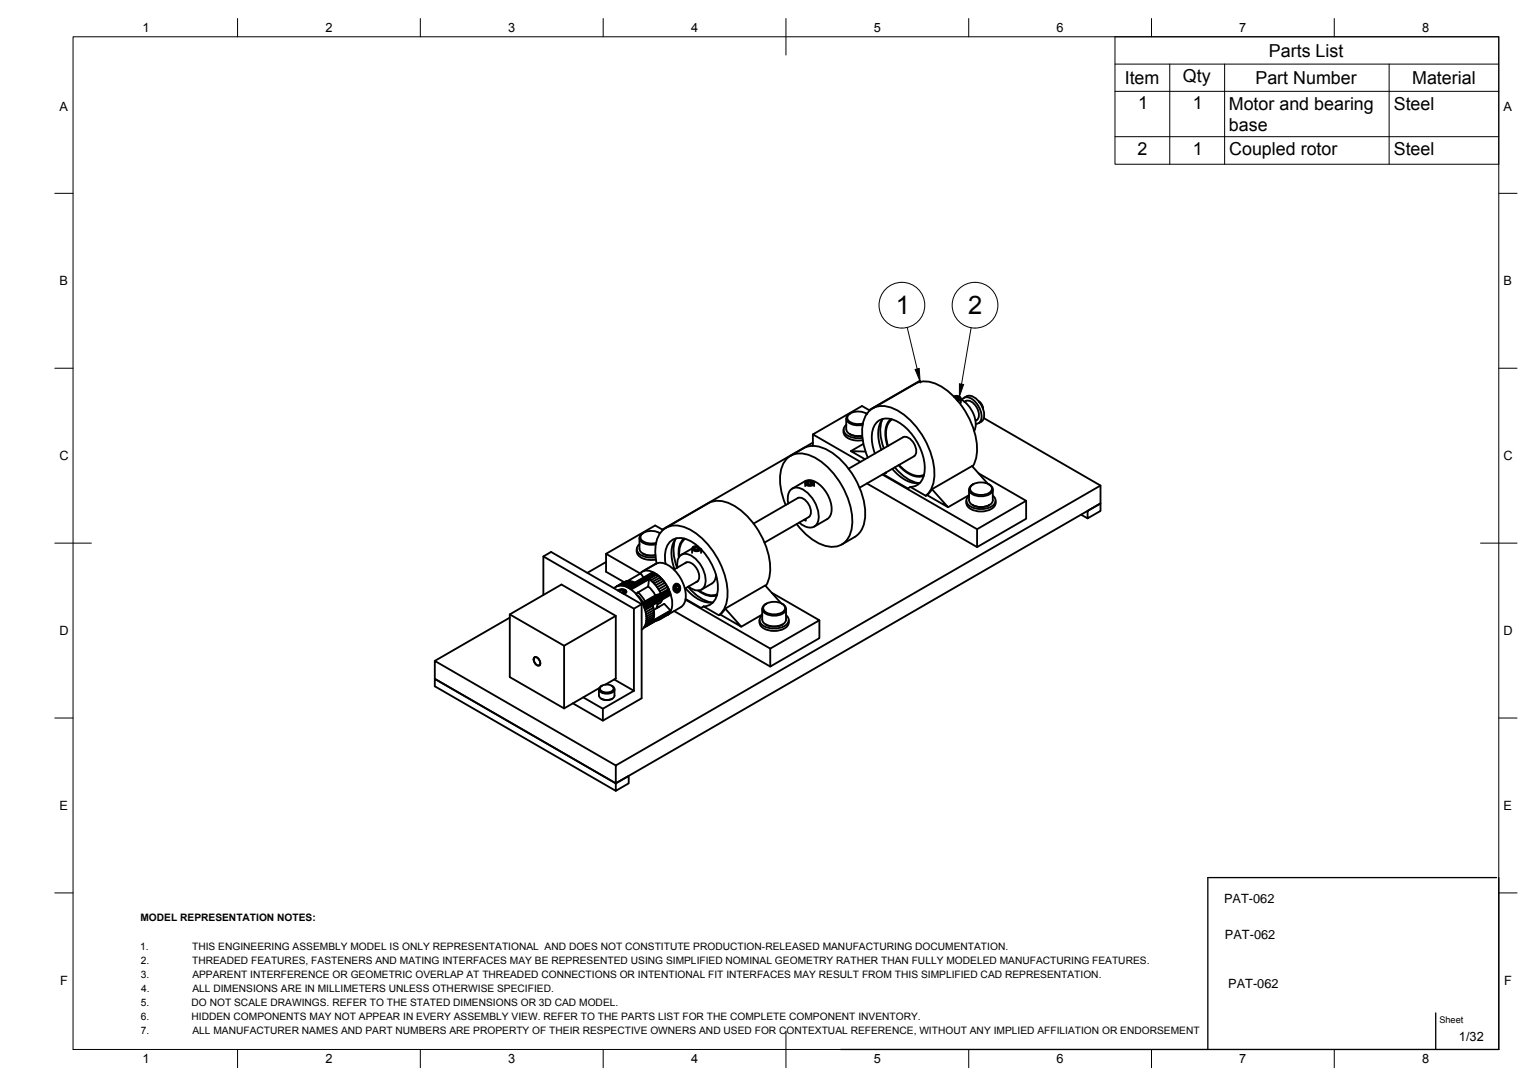
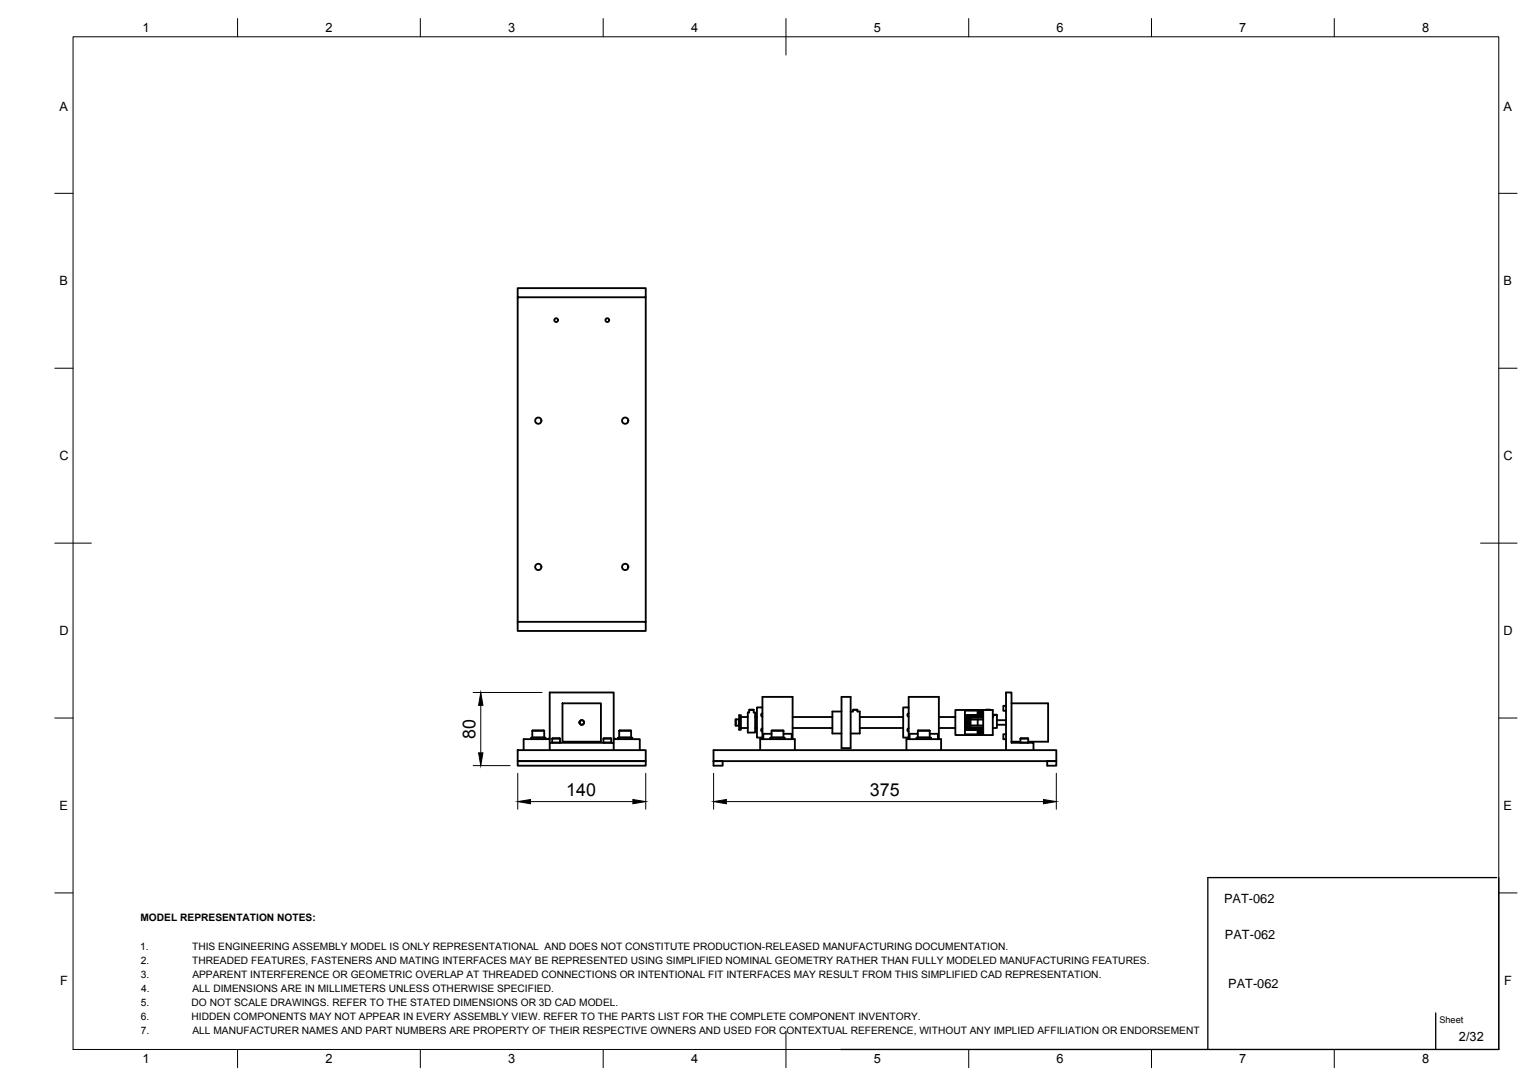
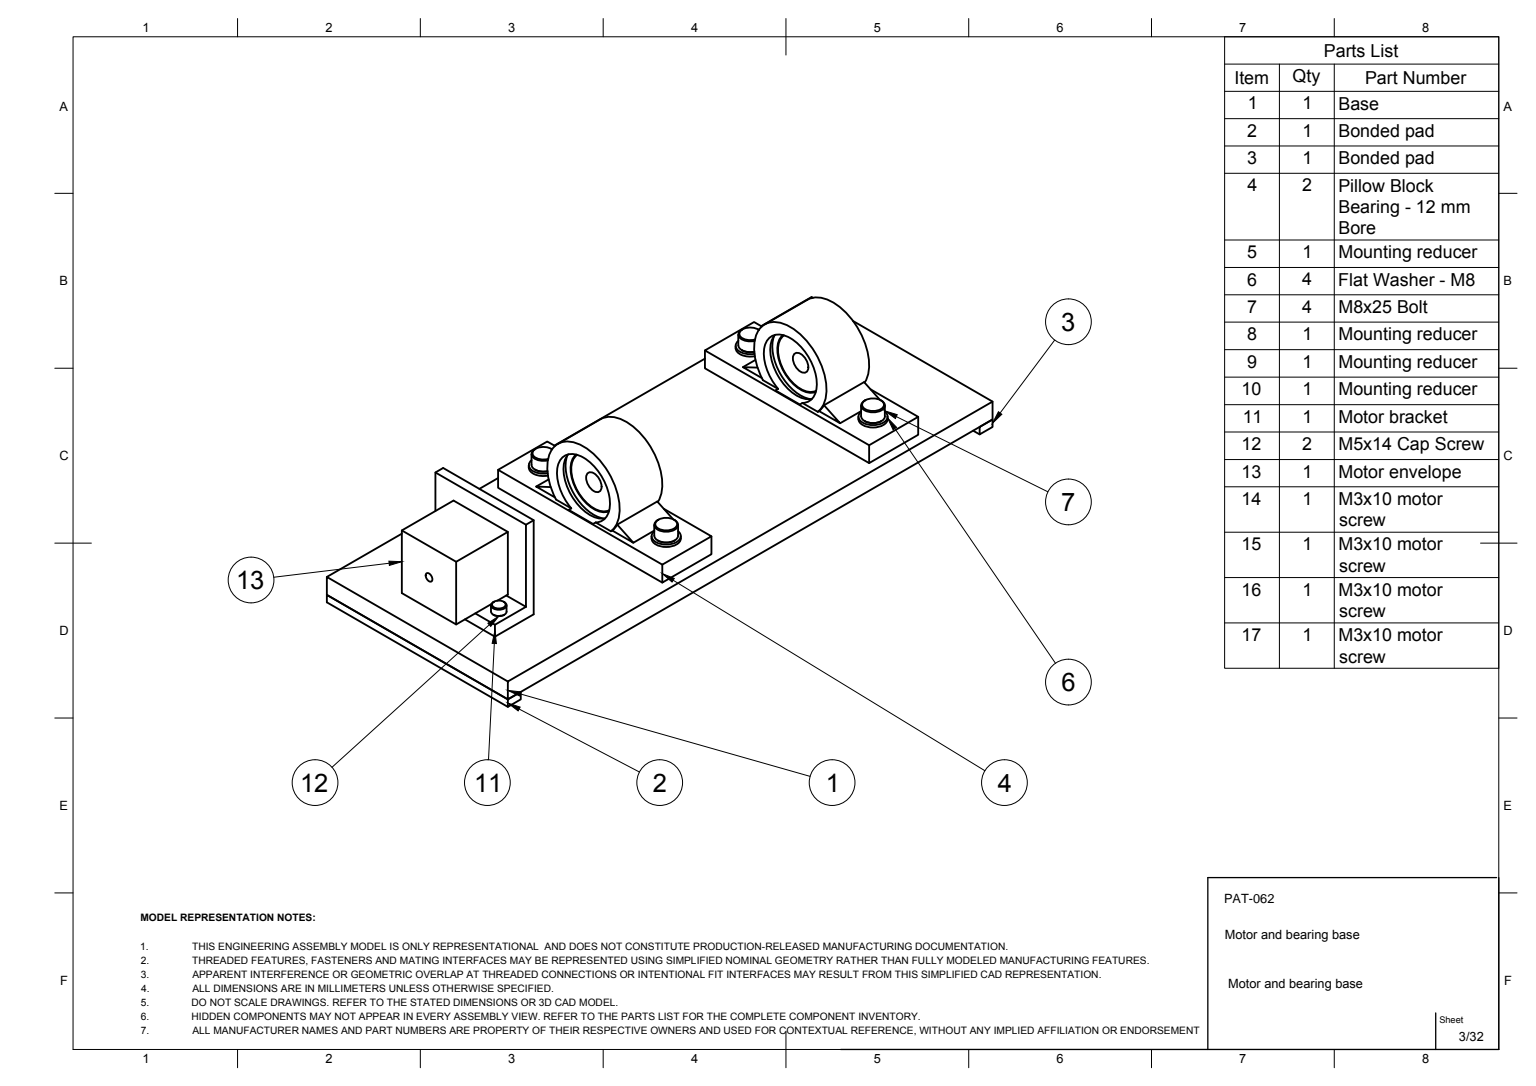
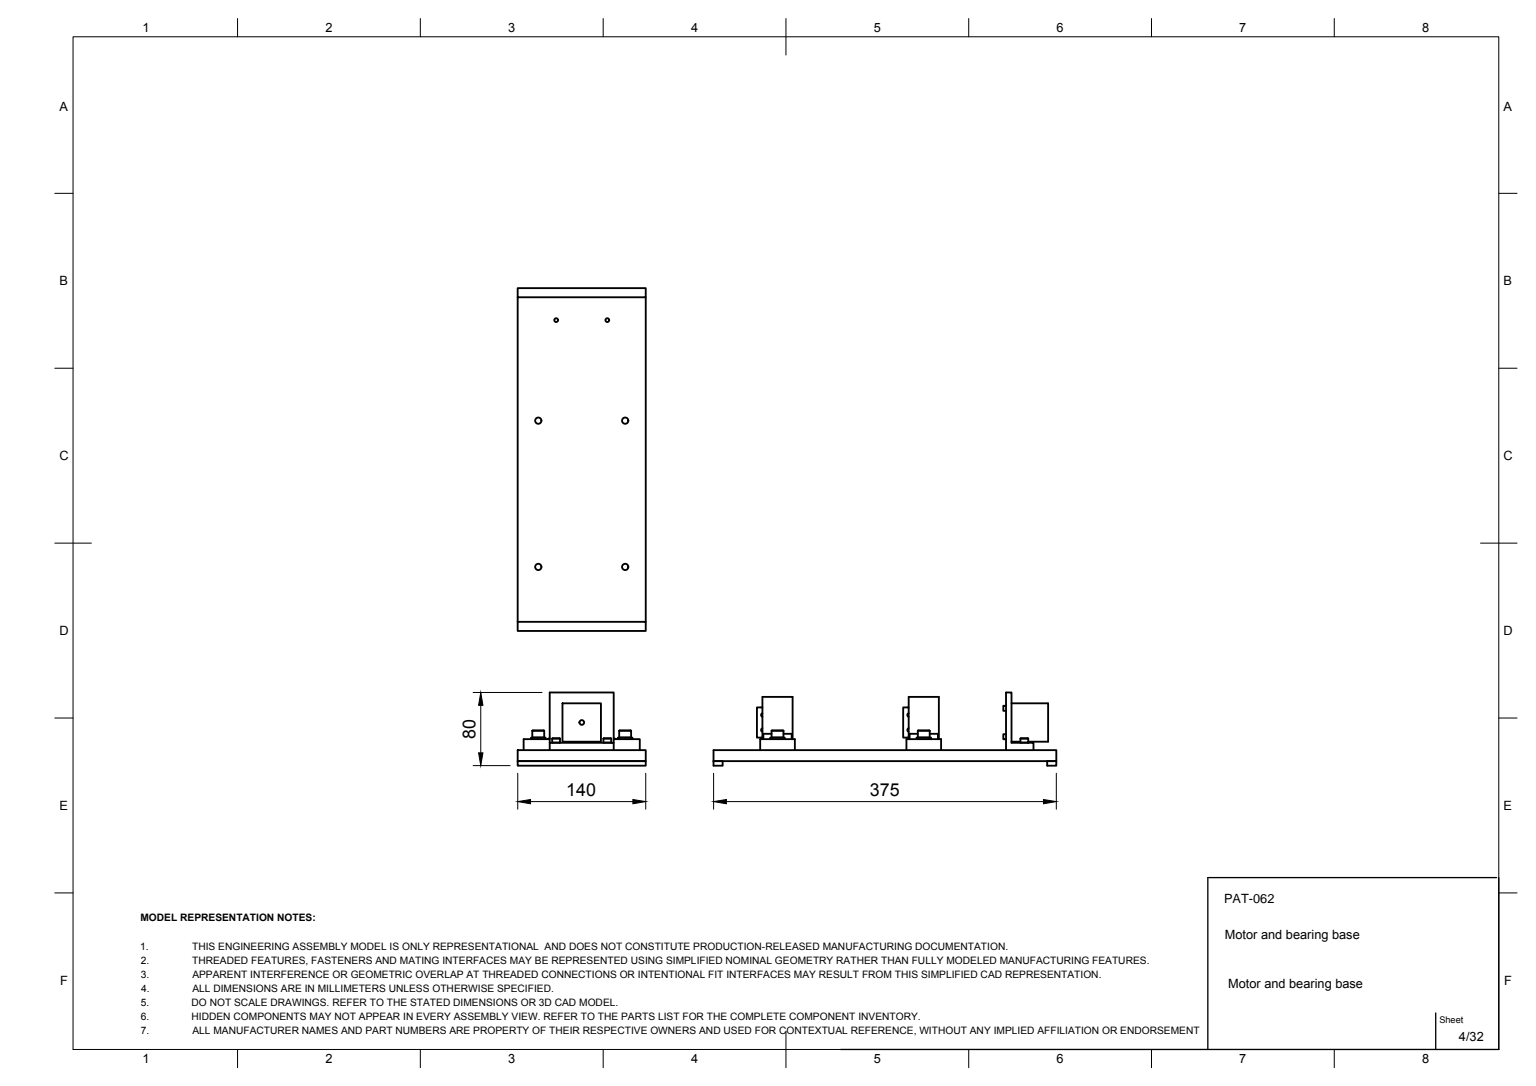
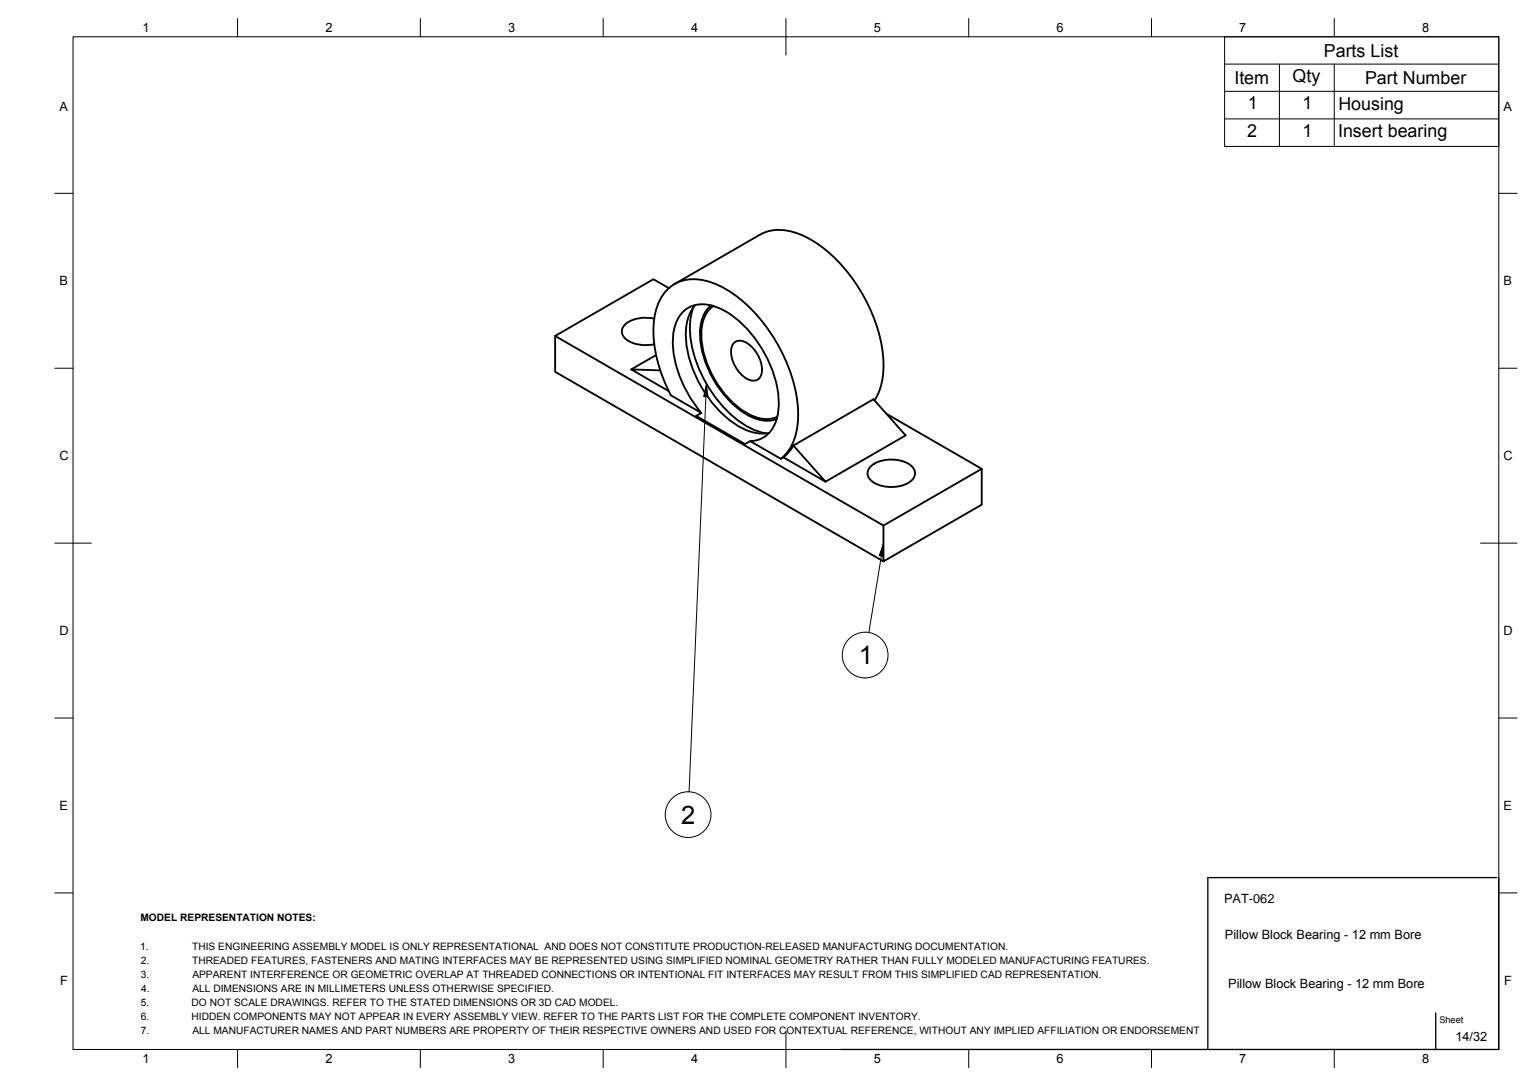
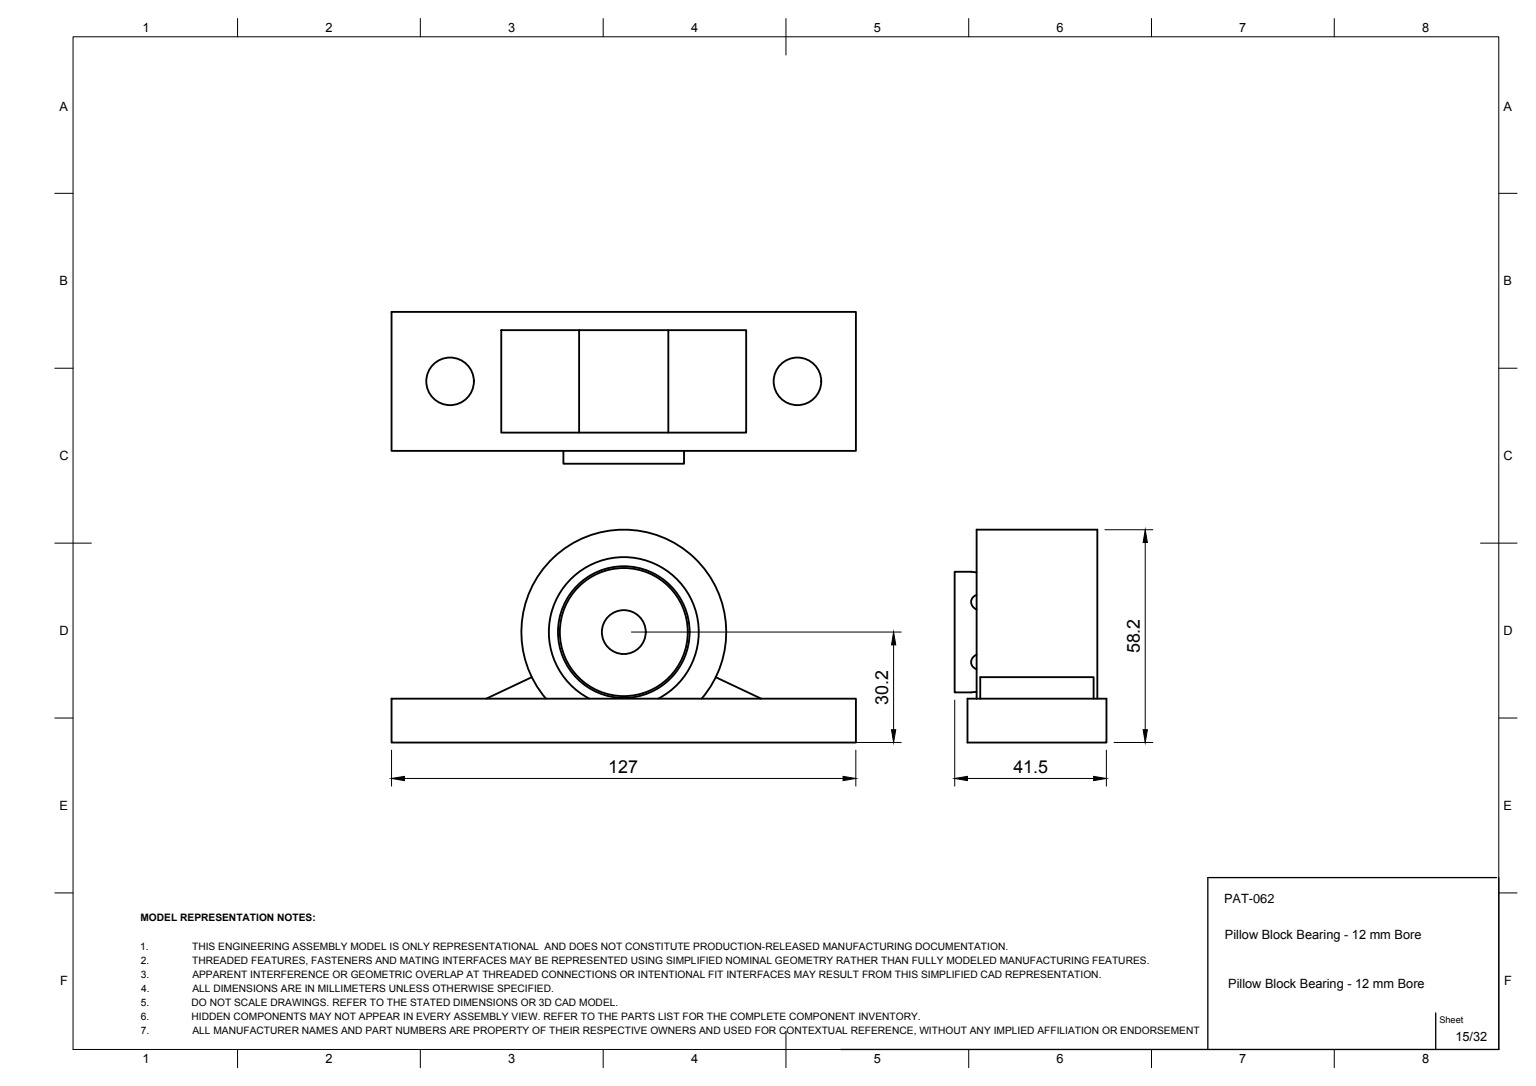
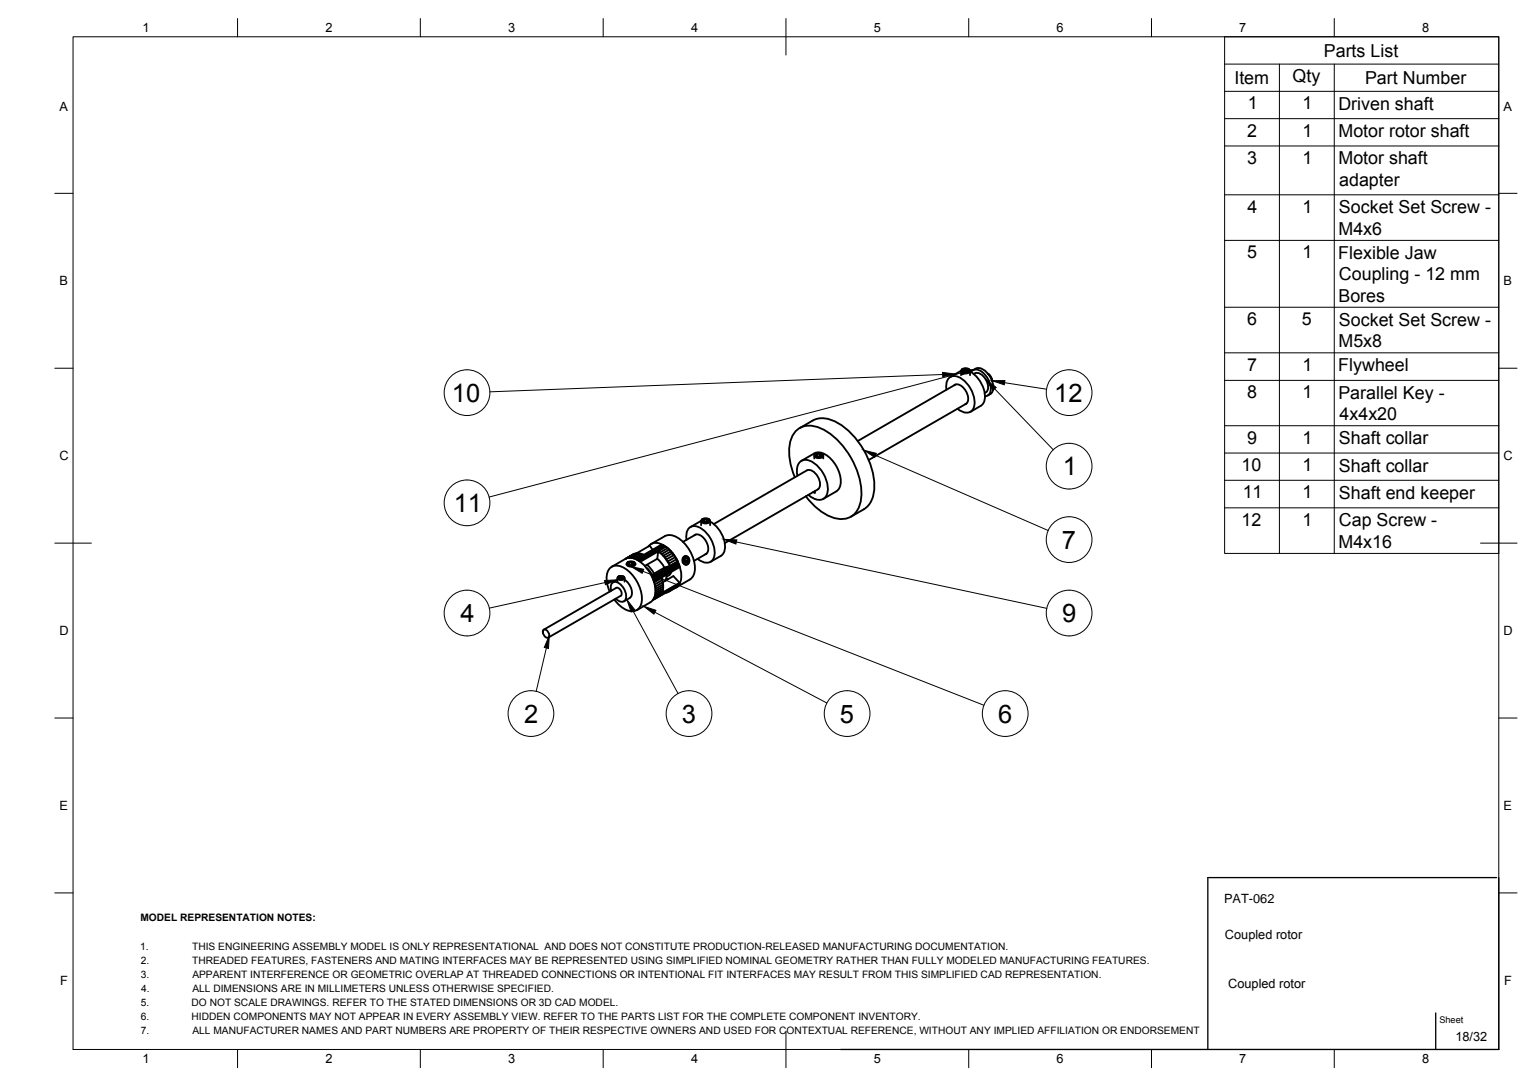
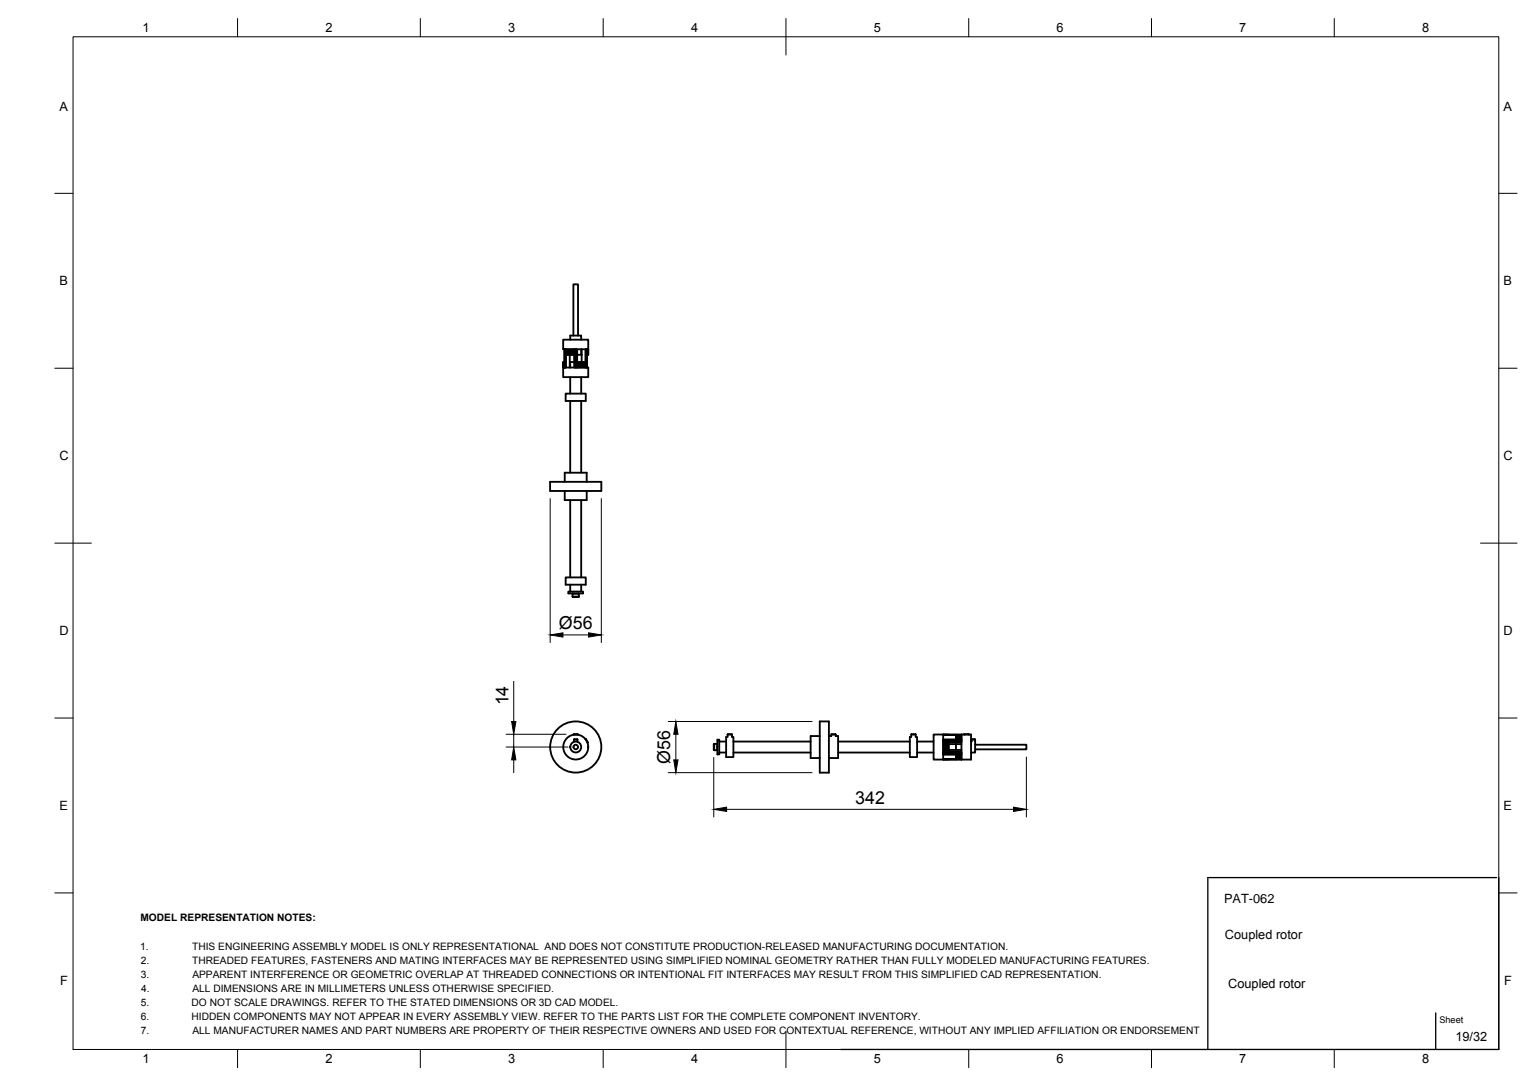
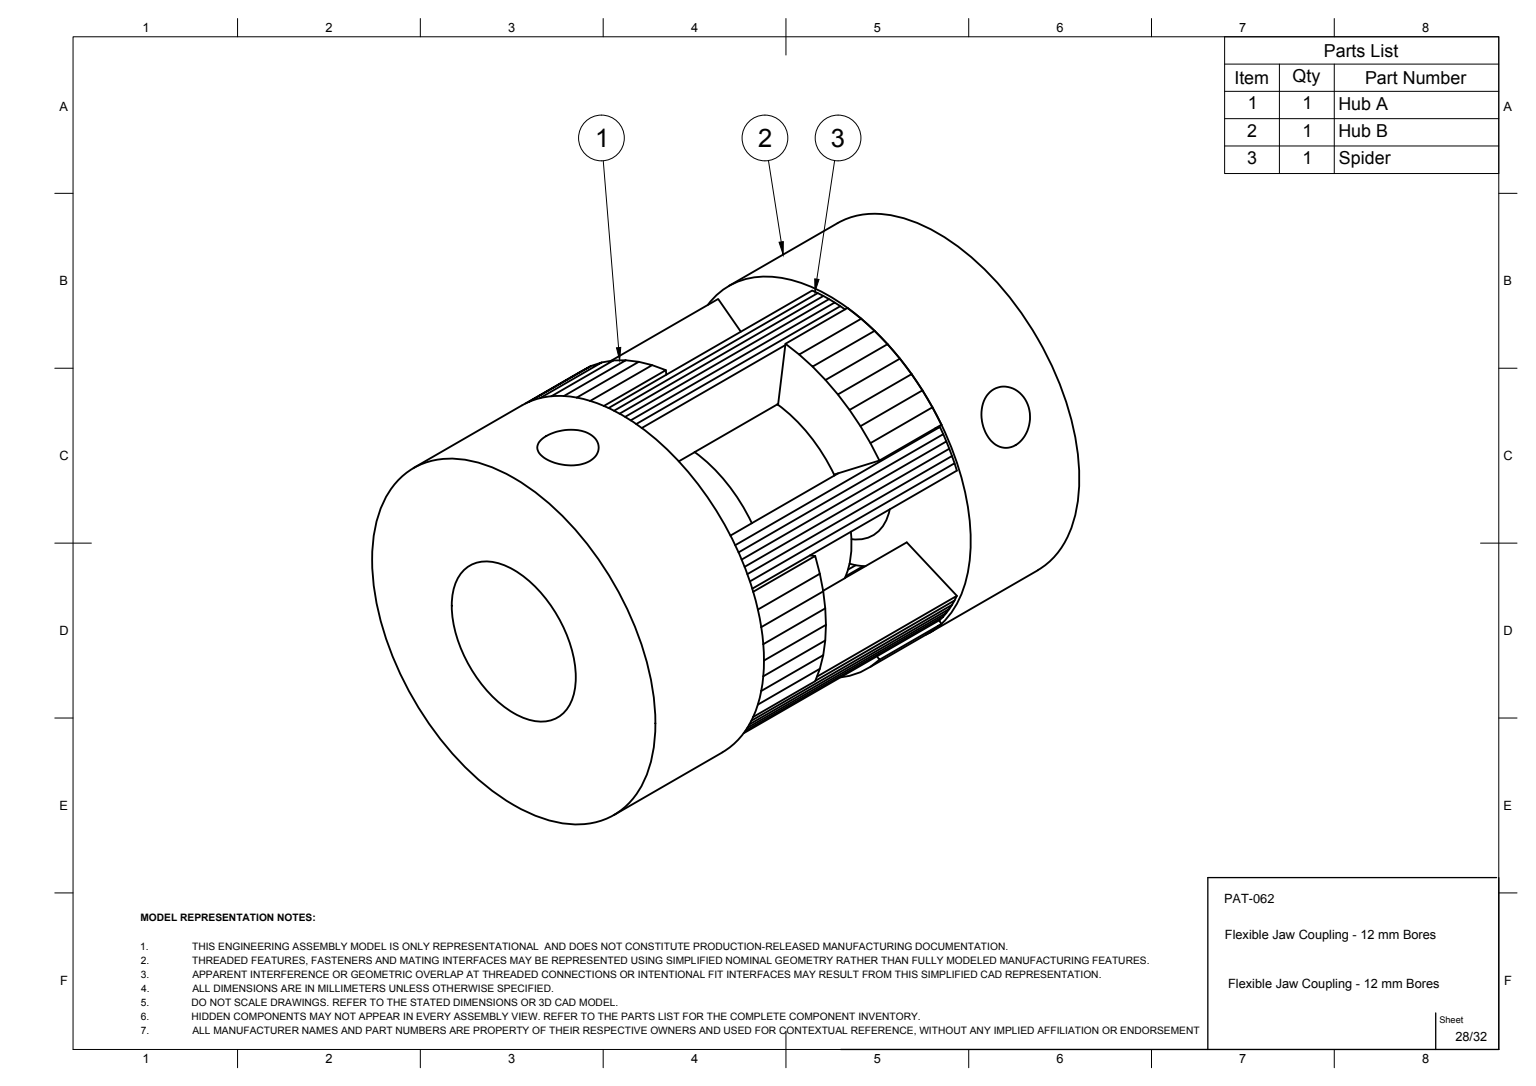
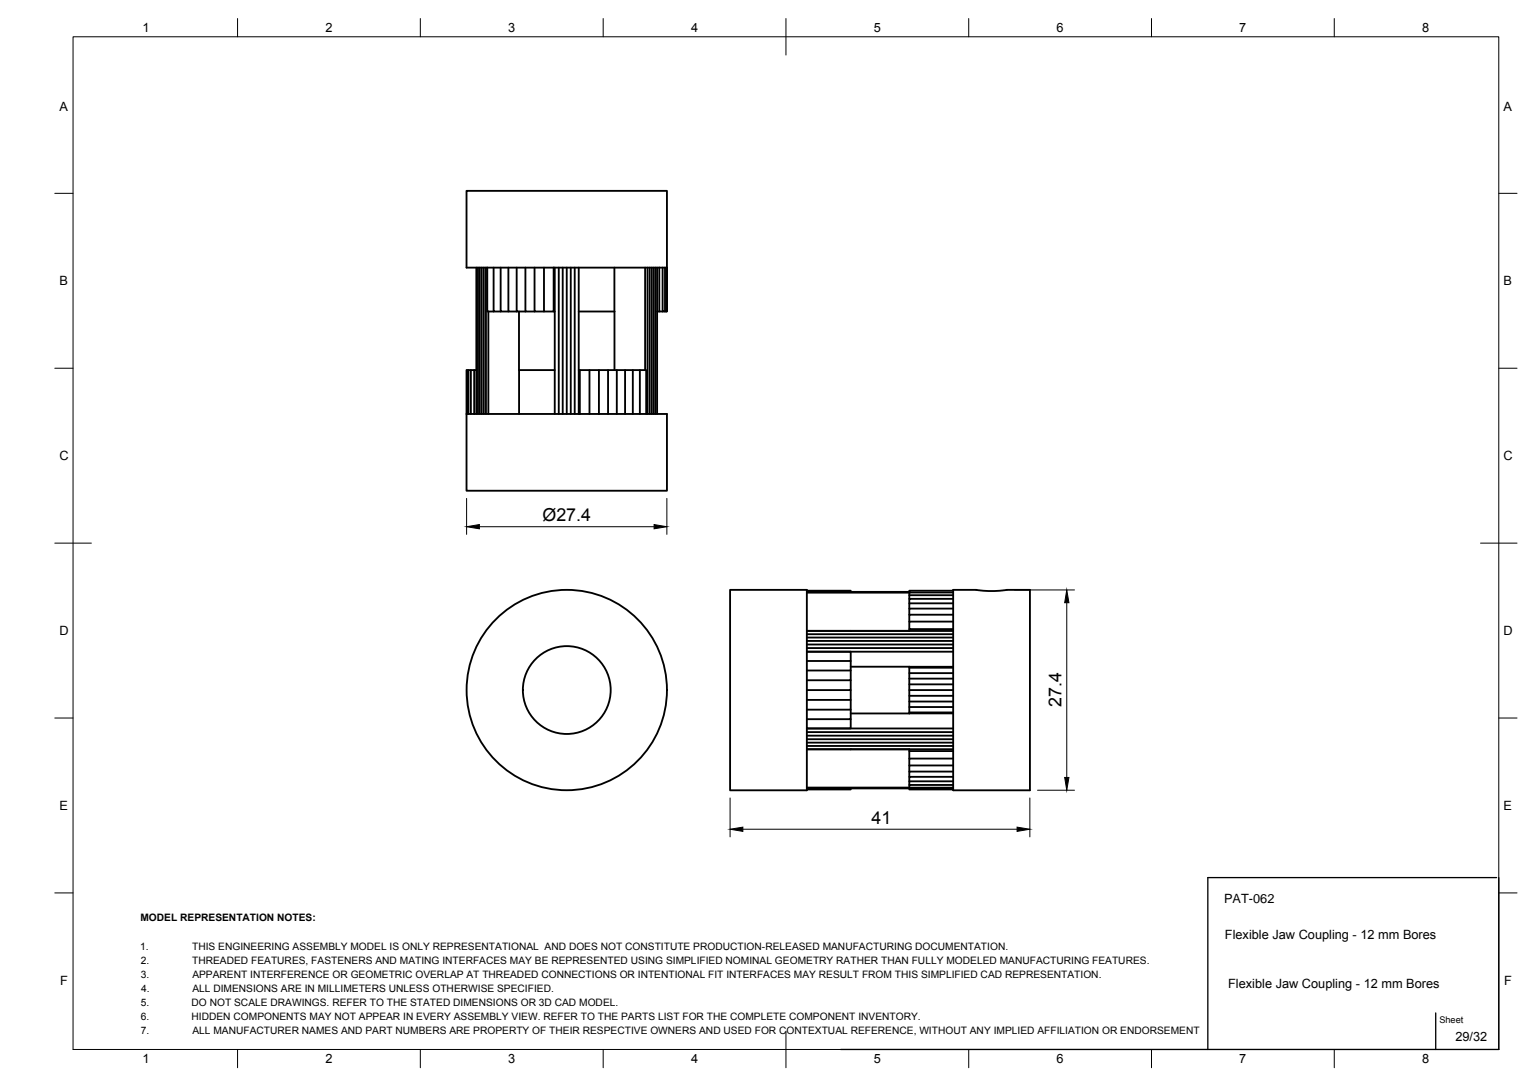
ISO-10303-21;
HEADER;
/* Generated by software containing ST-Developer
 * from STEP Tools, Inc. (www.steptools.com) 
 */

FILE_DESCRIPTION(
/* description */ ('Jaw-coupled motor to shaft test stand'),
/* implementation_level */ '2;1');

FILE_NAME(
/* name */ 'PAT-062',
/* time_stamp */ '2026-10-27T10:46:06-07:00',
/* author */ (''),
/* organization */ (''),
/* preprocessor_version */ 'ST-DEVELOPER v20.2',
/* originating_system */ 'Autodesk Translation Framework v15.17.0.0',
/* authorisation */ '');

FILE_SCHEMA (('AUTOMOTIVE_DESIGN { 1 0 10303 214 3 1 1 }'));
ENDSEC;

DATA;
#10=MECHANICAL_DESIGN_GEOMETRIC_PRESENTATION_REPRESENTATION('',(#340,#341,
#342,#343,#344,#345,#346,#347,#348,#349,#350,#351,#352,#353,#354,#355,#356,
#357,#358,#359,#360,#361,#362,#363,#364,#365,#366,#367,#368,#369,#370,#371,
#372),#19361);
#11=CONICAL_SURFACE('',#11682,0.625,0.785398163397448);
#12=CONICAL_SURFACE('',#11686,0.635,0.785398163397449);
#13=CONICAL_SURFACE('',#11690,0.41,0.463647609000806);
#14=CONICAL_SURFACE('',#11706,0.4,0.785398163397448);
#15=CONICAL_SURFACE('',#11710,0.41,0.785398163397448);
#16=CONICAL_SURFACE('',#11714,0.26,0.463647609000806);
#17=CONICAL_SURFACE('',#11856,0.185,0.785398163397449);
#18=CONICAL_SURFACE('',#11860,0.1625,0.785398163397449);
#19=CONICAL_SURFACE('',#12258,0.18,0.785398163397448);
#20=CONICAL_SURFACE('',#12262,0.18,0.785398163397448);
#21=CONICAL_SURFACE('',#12270,0.18,0.785398163397449);
#22=CONICAL_SURFACE('',#12273,0.18,0.785398163397449);
#23=CONICAL_SURFACE('',#12289,0.235,0.785398163397448);
#24=CONICAL_SURFACE('',#12293,0.2125,0.785398163397448);
#25=CONICAL_SURFACE('',#12299,0.325,0.785398163397448);
#26=CONICAL_SURFACE('',#12303,0.335,0.785398163397448);
#27=CONICAL_SURFACE('',#12307,0.21,0.463647609000806);
#28=CONICAL_SURFACE('',#12311,0.18,0.785398163397448);
#29=ORIENTED_CLOSED_SHELL('',*,#11001,.F.);
#30=ORIENTED_CLOSED_SHELL('',*,#11003,.F.);
#31=ORIENTED_CLOSED_SHELL('',*,#11019,.F.);
#32=BREP_WITH_VOIDS('Body1',#11002,(#29));
#33=BREP_WITH_VOIDS('Body1',#11004,(#30));
#34=BREP_WITH_VOIDS('Body1',#11018,(#31));
#35=ITEM_DEFINED_TRANSFORMATION($,$,#11579,#11658);
#36=ITEM_DEFINED_TRANSFORMATION($,$,#11630,#11659);
#37=ITEM_DEFINED_TRANSFORMATION($,$,#11375,#11717);
#38=ITEM_DEFINED_TRANSFORMATION($,$,#11400,#11718);
#39=ITEM_DEFINED_TRANSFORMATION($,$,#11407,#11719);
#40=ITEM_DEFINED_TRANSFORMATION($,$,#11414,#11720);
#41=ITEM_DEFINED_TRANSFORMATION($,$,#11423,#11721);
#42=ITEM_DEFINED_TRANSFORMATION($,$,#11432,#11722);
#43=ITEM_DEFINED_TRANSFORMATION($,$,#11441,#11723);
#44=ITEM_DEFINED_TRANSFORMATION($,$,#11450,#11724);
#45=ITEM_DEFINED_TRANSFORMATION($,$,#11480,#11725);
#46=ITEM_DEFINED_TRANSFORMATION($,$,#11510,#11726);
#47=ITEM_DEFINED_TRANSFORMATION($,$,#11527,#11727);
#48=ITEM_DEFINED_TRANSFORMATION($,$,#11544,#11728);
#49=ITEM_DEFINED_TRANSFORMATION($,$,#11561,#11729);
#50=ITEM_DEFINED_TRANSFORMATION($,$,#11578,#11730);
#51=ITEM_DEFINED_TRANSFORMATION($,$,#11660,#11731);
#52=ITEM_DEFINED_TRANSFORMATION($,$,#11669,#11732);
#53=ITEM_DEFINED_TRANSFORMATION($,$,#11660,#11733);
#54=ITEM_DEFINED_TRANSFORMATION($,$,#11669,#11734);
#55=ITEM_DEFINED_TRANSFORMATION($,$,#11578,#11735);
#56=ITEM_DEFINED_TRANSFORMATION($,$,#11660,#11736);
#57=ITEM_DEFINED_TRANSFORMATION($,$,#11669,#11737);
#58=ITEM_DEFINED_TRANSFORMATION($,$,#11660,#11738);
#59=ITEM_DEFINED_TRANSFORMATION($,$,#11669,#11739);
#60=ITEM_DEFINED_TRANSFORMATION($,$,#11693,#11740);
#61=ITEM_DEFINED_TRANSFORMATION($,$,#11693,#11741);
#62=ITEM_DEFINED_TRANSFORMATION($,$,#11864,#12253);
#63=ITEM_DEFINED_TRANSFORMATION($,$,#11982,#12254);
#64=ITEM_DEFINED_TRANSFORMATION($,$,#12100,#12255);
#65=ITEM_DEFINED_TRANSFORMATION($,$,#11743,#12322);
#66=ITEM_DEFINED_TRANSFORMATION($,$,#11760,#12323);
#67=ITEM_DEFINED_TRANSFORMATION($,$,#11766,#12324);
#68=ITEM_DEFINED_TRANSFORMATION($,$,#11781,#12325);
#69=ITEM_DEFINED_TRANSFORMATION($,$,#11807,#12326);
#70=ITEM_DEFINED_TRANSFORMATION($,$,#11822,#12327);
#71=ITEM_DEFINED_TRANSFORMATION($,$,#11837,#12328);
#72=ITEM_DEFINED_TRANSFORMATION($,$,#11846,#12329);
#73=ITEM_DEFINED_TRANSFORMATION($,$,#11863,#12330);
#74=ITEM_DEFINED_TRANSFORMATION($,$,#12279,#12331);
#75=ITEM_DEFINED_TRANSFORMATION($,$,#12279,#12332);
#76=ITEM_DEFINED_TRANSFORMATION($,$,#12256,#12333);
#77=ITEM_DEFINED_TRANSFORMATION($,$,#12279,#12334);
#78=ITEM_DEFINED_TRANSFORMATION($,$,#12279,#12335);
#79=ITEM_DEFINED_TRANSFORMATION($,$,#12279,#12336);
#80=ITEM_DEFINED_TRANSFORMATION($,$,#12296,#12337);
#81=ITEM_DEFINED_TRANSFORMATION($,$,#11374,#12338);
#82=ITEM_DEFINED_TRANSFORMATION($,$,#11742,#12339);
#83=(
REPRESENTATION_RELATIONSHIP($,$,#19504,#19503)
REPRESENTATION_RELATIONSHIP_WITH_TRANSFORMATION(#35)
SHAPE_REPRESENTATION_RELATIONSHIP()
);
#84=(
REPRESENTATION_RELATIONSHIP($,$,#19505,#19503)
REPRESENTATION_RELATIONSHIP_WITH_TRANSFORMATION(#36)
SHAPE_REPRESENTATION_RELATIONSHIP()
);
#85=(
REPRESENTATION_RELATIONSHIP($,$,#19490,#19489)
REPRESENTATION_RELATIONSHIP_WITH_TRANSFORMATION(#37)
SHAPE_REPRESENTATION_RELATIONSHIP()
);
#86=(
REPRESENTATION_RELATIONSHIP($,$,#19491,#19489)
REPRESENTATION_RELATIONSHIP_WITH_TRANSFORMATION(#38)
SHAPE_REPRESENTATION_RELATIONSHIP()
);
#87=(
REPRESENTATION_RELATIONSHIP($,$,#19492,#19489)
REPRESENTATION_RELATIONSHIP_WITH_TRANSFORMATION(#39)
SHAPE_REPRESENTATION_RELATIONSHIP()
);
#88=(
REPRESENTATION_RELATIONSHIP($,$,#19493,#19489)
REPRESENTATION_RELATIONSHIP_WITH_TRANSFORMATION(#40)
SHAPE_REPRESENTATION_RELATIONSHIP()
);
#89=(
REPRESENTATION_RELATIONSHIP($,$,#19494,#19489)
REPRESENTATION_RELATIONSHIP_WITH_TRANSFORMATION(#41)
SHAPE_REPRESENTATION_RELATIONSHIP()
);
#90=(
REPRESENTATION_RELATIONSHIP($,$,#19495,#19489)
REPRESENTATION_RELATIONSHIP_WITH_TRANSFORMATION(#42)
SHAPE_REPRESENTATION_RELATIONSHIP()
);
#91=(
REPRESENTATION_RELATIONSHIP($,$,#19496,#19489)
REPRESENTATION_RELATIONSHIP_WITH_TRANSFORMATION(#43)
SHAPE_REPRESENTATION_RELATIONSHIP()
);
#92=(
REPRESENTATION_RELATIONSHIP($,$,#19497,#19489)
REPRESENTATION_RELATIONSHIP_WITH_TRANSFORMATION(#44)
SHAPE_REPRESENTATION_RELATIONSHIP()
);
#93=(
REPRESENTATION_RELATIONSHIP($,$,#19498,#19489)
REPRESENTATION_RELATIONSHIP_WITH_TRANSFORMATION(#45)
SHAPE_REPRESENTATION_RELATIONSHIP()
);
#94=(
REPRESENTATION_RELATIONSHIP($,$,#19499,#19489)
REPRESENTATION_RELATIONSHIP_WITH_TRANSFORMATION(#46)
SHAPE_REPRESENTATION_RELATIONSHIP()
);
#95=(
REPRESENTATION_RELATIONSHIP($,$,#19500,#19489)
REPRESENTATION_RELATIONSHIP_WITH_TRANSFORMATION(#47)
SHAPE_REPRESENTATION_RELATIONSHIP()
);
#96=(
REPRESENTATION_RELATIONSHIP($,$,#19501,#19489)
REPRESENTATION_RELATIONSHIP_WITH_TRANSFORMATION(#48)
SHAPE_REPRESENTATION_RELATIONSHIP()
);
#97=(
REPRESENTATION_RELATIONSHIP($,$,#19502,#19489)
REPRESENTATION_RELATIONSHIP_WITH_TRANSFORMATION(#49)
SHAPE_REPRESENTATION_RELATIONSHIP()
);
#98=(
REPRESENTATION_RELATIONSHIP($,$,#19503,#19489)
REPRESENTATION_RELATIONSHIP_WITH_TRANSFORMATION(#50)
SHAPE_REPRESENTATION_RELATIONSHIP()
);
#99=(
REPRESENTATION_RELATIONSHIP($,$,#19506,#19489)
REPRESENTATION_RELATIONSHIP_WITH_TRANSFORMATION(#51)
SHAPE_REPRESENTATION_RELATIONSHIP()
);
#100=(
REPRESENTATION_RELATIONSHIP($,$,#19507,#19489)
REPRESENTATION_RELATIONSHIP_WITH_TRANSFORMATION(#52)
SHAPE_REPRESENTATION_RELATIONSHIP()
);
#101=(
REPRESENTATION_RELATIONSHIP($,$,#19506,#19489)
REPRESENTATION_RELATIONSHIP_WITH_TRANSFORMATION(#53)
SHAPE_REPRESENTATION_RELATIONSHIP()
);
#102=(
REPRESENTATION_RELATIONSHIP($,$,#19507,#19489)
REPRESENTATION_RELATIONSHIP_WITH_TRANSFORMATION(#54)
SHAPE_REPRESENTATION_RELATIONSHIP()
);
#103=(
REPRESENTATION_RELATIONSHIP($,$,#19503,#19489)
REPRESENTATION_RELATIONSHIP_WITH_TRANSFORMATION(#55)
SHAPE_REPRESENTATION_RELATIONSHIP()
);
#104=(
REPRESENTATION_RELATIONSHIP($,$,#19506,#19489)
REPRESENTATION_RELATIONSHIP_WITH_TRANSFORMATION(#56)
SHAPE_REPRESENTATION_RELATIONSHIP()
);
#105=(
REPRESENTATION_RELATIONSHIP($,$,#19507,#19489)
REPRESENTATION_RELATIONSHIP_WITH_TRANSFORMATION(#57)
SHAPE_REPRESENTATION_RELATIONSHIP()
);
#106=(
REPRESENTATION_RELATIONSHIP($,$,#19506,#19489)
REPRESENTATION_RELATIONSHIP_WITH_TRANSFORMATION(#58)
SHAPE_REPRESENTATION_RELATIONSHIP()
);
#107=(
REPRESENTATION_RELATIONSHIP($,$,#19507,#19489)
REPRESENTATION_RELATIONSHIP_WITH_TRANSFORMATION(#59)
SHAPE_REPRESENTATION_RELATIONSHIP()
);
#108=(
REPRESENTATION_RELATIONSHIP($,$,#19508,#19489)
REPRESENTATION_RELATIONSHIP_WITH_TRANSFORMATION(#60)
SHAPE_REPRESENTATION_RELATIONSHIP()
);
#109=(
REPRESENTATION_RELATIONSHIP($,$,#19508,#19489)
REPRESENTATION_RELATIONSHIP_WITH_TRANSFORMATION(#61)
SHAPE_REPRESENTATION_RELATIONSHIP()
);
#110=(
REPRESENTATION_RELATIONSHIP($,$,#19519,#19518)
REPRESENTATION_RELATIONSHIP_WITH_TRANSFORMATION(#62)
SHAPE_REPRESENTATION_RELATIONSHIP()
);
#111=(
REPRESENTATION_RELATIONSHIP($,$,#19520,#19518)
REPRESENTATION_RELATIONSHIP_WITH_TRANSFORMATION(#63)
SHAPE_REPRESENTATION_RELATIONSHIP()
);
#112=(
REPRESENTATION_RELATIONSHIP($,$,#19521,#19518)
REPRESENTATION_RELATIONSHIP_WITH_TRANSFORMATION(#64)
SHAPE_REPRESENTATION_RELATIONSHIP()
);
#113=(
REPRESENTATION_RELATIONSHIP($,$,#19510,#19509)
REPRESENTATION_RELATIONSHIP_WITH_TRANSFORMATION(#65)
SHAPE_REPRESENTATION_RELATIONSHIP()
);
#114=(
REPRESENTATION_RELATIONSHIP($,$,#19511,#19509)
REPRESENTATION_RELATIONSHIP_WITH_TRANSFORMATION(#66)
SHAPE_REPRESENTATION_RELATIONSHIP()
);
#115=(
REPRESENTATION_RELATIONSHIP($,$,#19512,#19509)
REPRESENTATION_RELATIONSHIP_WITH_TRANSFORMATION(#67)
SHAPE_REPRESENTATION_RELATIONSHIP()
);
#116=(
REPRESENTATION_RELATIONSHIP($,$,#19513,#19509)
REPRESENTATION_RELATIONSHIP_WITH_TRANSFORMATION(#68)
SHAPE_REPRESENTATION_RELATIONSHIP()
);
#117=(
REPRESENTATION_RELATIONSHIP($,$,#19514,#19509)
REPRESENTATION_RELATIONSHIP_WITH_TRANSFORMATION(#69)
SHAPE_REPRESENTATION_RELATIONSHIP()
);
#118=(
REPRESENTATION_RELATIONSHIP($,$,#19515,#19509)
REPRESENTATION_RELATIONSHIP_WITH_TRANSFORMATION(#70)
SHAPE_REPRESENTATION_RELATIONSHIP()
);
#119=(
REPRESENTATION_RELATIONSHIP($,$,#19516,#19509)
REPRESENTATION_RELATIONSHIP_WITH_TRANSFORMATION(#71)
SHAPE_REPRESENTATION_RELATIONSHIP()
);
#120=(
REPRESENTATION_RELATIONSHIP($,$,#19517,#19509)
REPRESENTATION_RELATIONSHIP_WITH_TRANSFORMATION(#72)
SHAPE_REPRESENTATION_RELATIONSHIP()
);
#121=(
REPRESENTATION_RELATIONSHIP($,$,#19518,#19509)
REPRESENTATION_RELATIONSHIP_WITH_TRANSFORMATION(#73)
SHAPE_REPRESENTATION_RELATIONSHIP()
);
#122=(
REPRESENTATION_RELATIONSHIP($,$,#19523,#19509)
REPRESENTATION_RELATIONSHIP_WITH_TRANSFORMATION(#74)
SHAPE_REPRESENTATION_RELATIONSHIP()
);
#123=(
REPRESENTATION_RELATIONSHIP($,$,#19523,#19509)
REPRESENTATION_RELATIONSHIP_WITH_TRANSFORMATION(#75)
SHAPE_REPRESENTATION_RELATIONSHIP()
);
#124=(
REPRESENTATION_RELATIONSHIP($,$,#19522,#19509)
REPRESENTATION_RELATIONSHIP_WITH_TRANSFORMATION(#76)
SHAPE_REPRESENTATION_RELATIONSHIP()
);
#125=(
REPRESENTATION_RELATIONSHIP($,$,#19523,#19509)
REPRESENTATION_RELATIONSHIP_WITH_TRANSFORMATION(#77)
SHAPE_REPRESENTATION_RELATIONSHIP()
);
#126=(
REPRESENTATION_RELATIONSHIP($,$,#19523,#19509)
REPRESENTATION_RELATIONSHIP_WITH_TRANSFORMATION(#78)
SHAPE_REPRESENTATION_RELATIONSHIP()
);
#127=(
REPRESENTATION_RELATIONSHIP($,$,#19523,#19509)
REPRESENTATION_RELATIONSHIP_WITH_TRANSFORMATION(#79)
SHAPE_REPRESENTATION_RELATIONSHIP()
);
#128=(
REPRESENTATION_RELATIONSHIP($,$,#19524,#19509)
REPRESENTATION_RELATIONSHIP_WITH_TRANSFORMATION(#80)
SHAPE_REPRESENTATION_RELATIONSHIP()
);
#129=(
REPRESENTATION_RELATIONSHIP($,$,#19489,#19488)
REPRESENTATION_RELATIONSHIP_WITH_TRANSFORMATION(#81)
SHAPE_REPRESENTATION_RELATIONSHIP()
);
#130=(
REPRESENTATION_RELATIONSHIP($,$,#19509,#19488)
REPRESENTATION_RELATIONSHIP_WITH_TRANSFORMATION(#82)
SHAPE_REPRESENTATION_RELATIONSHIP()
);
#131=CONTEXT_DEPENDENT_SHAPE_REPRESENTATION(#83,#19421);
#132=CONTEXT_DEPENDENT_SHAPE_REPRESENTATION(#84,#19422);
#133=CONTEXT_DEPENDENT_SHAPE_REPRESENTATION(#85,#19426);
#134=CONTEXT_DEPENDENT_SHAPE_REPRESENTATION(#86,#19427);
#135=CONTEXT_DEPENDENT_SHAPE_REPRESENTATION(#87,#19428);
#136=CONTEXT_DEPENDENT_SHAPE_REPRESENTATION(#88,#19429);
#137=CONTEXT_DEPENDENT_SHAPE_REPRESENTATION(#89,#19430);
#138=CONTEXT_DEPENDENT_SHAPE_REPRESENTATION(#90,#19431);
#139=CONTEXT_DEPENDENT_SHAPE_REPRESENTATION(#91,#19432);
#140=CONTEXT_DEPENDENT_SHAPE_REPRESENTATION(#92,#19433);
#141=CONTEXT_DEPENDENT_SHAPE_REPRESENTATION(#93,#19434);
#142=CONTEXT_DEPENDENT_SHAPE_REPRESENTATION(#94,#19435);
#143=CONTEXT_DEPENDENT_SHAPE_REPRESENTATION(#95,#19436);
#144=CONTEXT_DEPENDENT_SHAPE_REPRESENTATION(#96,#19437);
#145=CONTEXT_DEPENDENT_SHAPE_REPRESENTATION(#97,#19438);
#146=CONTEXT_DEPENDENT_SHAPE_REPRESENTATION(#98,#19439);
#147=CONTEXT_DEPENDENT_SHAPE_REPRESENTATION(#99,#19440);
#148=CONTEXT_DEPENDENT_SHAPE_REPRESENTATION(#100,#19441);
#149=CONTEXT_DEPENDENT_SHAPE_REPRESENTATION(#101,#19442);
#150=CONTEXT_DEPENDENT_SHAPE_REPRESENTATION(#102,#19443);
#151=CONTEXT_DEPENDENT_SHAPE_REPRESENTATION(#103,#19444);
#152=CONTEXT_DEPENDENT_SHAPE_REPRESENTATION(#104,#19445);
#153=CONTEXT_DEPENDENT_SHAPE_REPRESENTATION(#105,#19446);
#154=CONTEXT_DEPENDENT_SHAPE_REPRESENTATION(#106,#19447);
#155=CONTEXT_DEPENDENT_SHAPE_REPRESENTATION(#107,#19448);
#156=CONTEXT_DEPENDENT_SHAPE_REPRESENTATION(#108,#19449);
#157=CONTEXT_DEPENDENT_SHAPE_REPRESENTATION(#109,#19450);
#158=CONTEXT_DEPENDENT_SHAPE_REPRESENTATION(#110,#19464);
#159=CONTEXT_DEPENDENT_SHAPE_REPRESENTATION(#111,#19465);
#160=CONTEXT_DEPENDENT_SHAPE_REPRESENTATION(#112,#19466);
#161=CONTEXT_DEPENDENT_SHAPE_REPRESENTATION(#113,#19470);
#162=CONTEXT_DEPENDENT_SHAPE_REPRESENTATION(#114,#19471);
#163=CONTEXT_DEPENDENT_SHAPE_REPRESENTATION(#115,#19472);
#164=CONTEXT_DEPENDENT_SHAPE_REPRESENTATION(#116,#19473);
#165=CONTEXT_DEPENDENT_SHAPE_REPRESENTATION(#117,#19474);
#166=CONTEXT_DEPENDENT_SHAPE_REPRESENTATION(#118,#19475);
#167=CONTEXT_DEPENDENT_SHAPE_REPRESENTATION(#119,#19476);
#168=CONTEXT_DEPENDENT_SHAPE_REPRESENTATION(#120,#19477);
#169=CONTEXT_DEPENDENT_SHAPE_REPRESENTATION(#121,#19478);
#170=CONTEXT_DEPENDENT_SHAPE_REPRESENTATION(#122,#19479);
#171=CONTEXT_DEPENDENT_SHAPE_REPRESENTATION(#123,#19480);
#172=CONTEXT_DEPENDENT_SHAPE_REPRESENTATION(#124,#19481);
#173=CONTEXT_DEPENDENT_SHAPE_REPRESENTATION(#125,#19482);
#174=CONTEXT_DEPENDENT_SHAPE_REPRESENTATION(#126,#19483);
#175=CONTEXT_DEPENDENT_SHAPE_REPRESENTATION(#127,#19484);
#176=CONTEXT_DEPENDENT_SHAPE_REPRESENTATION(#128,#19485);
#177=CONTEXT_DEPENDENT_SHAPE_REPRESENTATION(#129,#19486);
#178=CONTEXT_DEPENDENT_SHAPE_REPRESENTATION(#130,#19487);
#179=NEXT_ASSEMBLY_USAGE_OCCURRENCE('Housing:1','Housing:1','Housing:1',
#19541,#19542,'Housing:1');
#180=NEXT_ASSEMBLY_USAGE_OCCURRENCE('Insert bearing:1',
'Insert bearing:1','Insert bearing:1',#19541,#19543,'Insert bearing:1');
#181=NEXT_ASSEMBLY_USAGE_OCCURRENCE('Base:1','Base:1','Base:1',#19527,#19528,
'Base:1');
#182=NEXT_ASSEMBLY_USAGE_OCCURRENCE('Bonded pad:1','Bonded pad:1',
'Bonded pad:1',#19527,#19529,'Bonded pad:1');
#183=NEXT_ASSEMBLY_USAGE_OCCURRENCE('Bonded pad (1):1',
'Bonded pad (1):1','Bonded pad (1):1',#19527,#19530,'Bonded pad (1):1');
#184=NEXT_ASSEMBLY_USAGE_OCCURRENCE('Mounting reducer:1',
'Mounting reducer:1','Mounting reducer:1',#19527,#19531,
'Mounting reducer:1');
#185=NEXT_ASSEMBLY_USAGE_OCCURRENCE('Mounting reducer (1):1',
'Mounting reducer (1):1','Mounting reducer (1):1',#19527,#19532,
'Mounting reducer (1):1');
#186=NEXT_ASSEMBLY_USAGE_OCCURRENCE('Mounting reducer (2):1',
'Mounting reducer (2):1','Mounting reducer (2):1',#19527,#19533,
'Mounting reducer (2):1');
#187=NEXT_ASSEMBLY_USAGE_OCCURRENCE('Mounting reducer (3):1',
'Mounting reducer (3):1','Mounting reducer (3):1',#19527,#19534,
'Mounting reducer (3):1');
#188=NEXT_ASSEMBLY_USAGE_OCCURRENCE('Motor bracket:1','Motor bracket:1',
'Motor bracket:1',#19527,#19535,'Motor bracket:1');
#189=NEXT_ASSEMBLY_USAGE_OCCURRENCE('Motor envelope:1',
'Motor envelope:1','Motor envelope:1',#19527,#19536,'Motor envelope:1');
#190=NEXT_ASSEMBLY_USAGE_OCCURRENCE('M3x10 motor screw:1',
'M3x10 motor screw:1','M3x10 motor screw:1',#19527,#19537,
'M3x10 motor screw:1');
#191=NEXT_ASSEMBLY_USAGE_OCCURRENCE('M3x10 motor screw (1):1',
'M3x10 motor screw (1):1','M3x10 motor screw (1):1',#19527,#19538,
'M3x10 motor screw (1):1');
#192=NEXT_ASSEMBLY_USAGE_OCCURRENCE('M3x10 motor screw (2):1',
'M3x10 motor screw (2):1','M3x10 motor screw (2):1',#19527,#19539,
'M3x10 motor screw (2):1');
#193=NEXT_ASSEMBLY_USAGE_OCCURRENCE('M3x10 motor screw (3):1',
'M3x10 motor screw (3):1','M3x10 motor screw (3):1',#19527,#19540,
'M3x10 motor screw (3):1');
#194=NEXT_ASSEMBLY_USAGE_OCCURRENCE(
'Pillow Block Bearing - 12 mm Bore:2',
'Pillow Block Bearing - 12 mm Bore:2',
'Pillow Block Bearing - 12 mm Bore:2',#19527,#19541,
'Pillow Block Bearing - 12 mm Bore:2');
#195=NEXT_ASSEMBLY_USAGE_OCCURRENCE('Flat Washer - M8:2',
'Flat Washer - M8:2','Flat Washer - M8:2',#19527,#19544,
'Flat Washer - M8:2');
#196=NEXT_ASSEMBLY_USAGE_OCCURRENCE('M8x25 Bolt:2','M8x25 Bolt:2',
'M8x25 Bolt:2',#19527,#19545,'M8x25 Bolt:2');
#197=NEXT_ASSEMBLY_USAGE_OCCURRENCE('Flat Washer - M8:3',
'Flat Washer - M8:3','Flat Washer - M8:3',#19527,#19544,
'Flat Washer - M8:3');
#198=NEXT_ASSEMBLY_USAGE_OCCURRENCE('M8x25 Bolt:3','M8x25 Bolt:3',
'M8x25 Bolt:3',#19527,#19545,'M8x25 Bolt:3');
#199=NEXT_ASSEMBLY_USAGE_OCCURRENCE(
'Pillow Block Bearing - 12 mm Bore:3',
'Pillow Block Bearing - 12 mm Bore:3',
'Pillow Block Bearing - 12 mm Bore:3',#19527,#19541,
'Pillow Block Bearing - 12 mm Bore:3');
#200=NEXT_ASSEMBLY_USAGE_OCCURRENCE('Flat Washer - M8:4',
'Flat Washer - M8:4','Flat Washer - M8:4',#19527,#19544,
'Flat Washer - M8:4');
#201=NEXT_ASSEMBLY_USAGE_OCCURRENCE('M8x25 Bolt:4','M8x25 Bolt:4',
'M8x25 Bolt:4',#19527,#19545,'M8x25 Bolt:4');
#202=NEXT_ASSEMBLY_USAGE_OCCURRENCE('Flat Washer - M8:5',
'Flat Washer - M8:5','Flat Washer - M8:5',#19527,#19544,
'Flat Washer - M8:5');
#203=NEXT_ASSEMBLY_USAGE_OCCURRENCE('M8x25 Bolt:5','M8x25 Bolt:5',
'M8x25 Bolt:5',#19527,#19545,'M8x25 Bolt:5');
#204=NEXT_ASSEMBLY_USAGE_OCCURRENCE('M5x14 Cap Screw:2',
'M5x14 Cap Screw:2','M5x14 Cap Screw:2',#19527,#19546,
'M5x14 Cap Screw:2');
#205=NEXT_ASSEMBLY_USAGE_OCCURRENCE('M5x14 Cap Screw:3',
'M5x14 Cap Screw:3','M5x14 Cap Screw:3',#19527,#19546,
'M5x14 Cap Screw:3');
#206=NEXT_ASSEMBLY_USAGE_OCCURRENCE('Hub A:1','Hub A:1','Hub A:1',#19556,
#19557,'Hub A:1');
#207=NEXT_ASSEMBLY_USAGE_OCCURRENCE('Hub B:1','Hub B:1','Hub B:1',#19556,
#19558,'Hub B:1');
#208=NEXT_ASSEMBLY_USAGE_OCCURRENCE('Spider:1','Spider:1','Spider:1',#19556,
#19559,'Spider:1');
#209=NEXT_ASSEMBLY_USAGE_OCCURRENCE('Driven shaft:1','Driven shaft:1',
'Driven shaft:1',#19547,#19548,'Driven shaft:1');
#210=NEXT_ASSEMBLY_USAGE_OCCURRENCE('Motor rotor shaft:1',
'Motor rotor shaft:1','Motor rotor shaft:1',#19547,#19549,
'Motor rotor shaft:1');
#211=NEXT_ASSEMBLY_USAGE_OCCURRENCE('Motor shaft adapter:1',
'Motor shaft adapter:1','Motor shaft adapter:1',#19547,#19550,
'Motor shaft adapter:1');
#212=NEXT_ASSEMBLY_USAGE_OCCURRENCE('Flywheel:1','Flywheel:1',
'Flywheel:1',#19547,#19551,'Flywheel:1');
#213=NEXT_ASSEMBLY_USAGE_OCCURRENCE('Shaft collar:1','Shaft collar:1',
'Shaft collar:1',#19547,#19552,'Shaft collar:1');
#214=NEXT_ASSEMBLY_USAGE_OCCURRENCE('Shaft collar (1):1',
'Shaft collar (1):1','Shaft collar (1):1',#19547,#19553,
'Shaft collar (1):1');
#215=NEXT_ASSEMBLY_USAGE_OCCURRENCE('Shaft end keeper:1',
'Shaft end keeper:1','Shaft end keeper:1',#19547,#19554,
'Shaft end keeper:1');
#216=NEXT_ASSEMBLY_USAGE_OCCURRENCE('Socket Set Screw - M4x6:2',
'Socket Set Screw - M4x6:2','Socket Set Screw - M4x6:2',#19547,#19555,
'Socket Set Screw - M4x6:2');
#217=NEXT_ASSEMBLY_USAGE_OCCURRENCE(
'Flexible Jaw Coupling - 12 mm Bores:2',
'Flexible Jaw Coupling - 12 mm Bores:2',
'Flexible Jaw Coupling - 12 mm Bores:2',#19547,#19556,
'Flexible Jaw Coupling - 12 mm Bores:2');
#218=NEXT_ASSEMBLY_USAGE_OCCURRENCE('Socket Set Screw - M5x8:2',
'Socket Set Screw - M5x8:2','Socket Set Screw - M5x8:2',#19547,#19561,
'Socket Set Screw - M5x8:2');
#219=NEXT_ASSEMBLY_USAGE_OCCURRENCE('Socket Set Screw - M5x8:3',
'Socket Set Screw - M5x8:3','Socket Set Screw - M5x8:3',#19547,#19561,
'Socket Set Screw - M5x8:3');
#220=NEXT_ASSEMBLY_USAGE_OCCURRENCE('Parallel Key - 4x4x20:2',
'Parallel Key - 4x4x20:2','Parallel Key - 4x4x20:2',#19547,#19560,
'Parallel Key - 4x4x20:2');
#221=NEXT_ASSEMBLY_USAGE_OCCURRENCE('Socket Set Screw - M5x8:4',
'Socket Set Screw - M5x8:4','Socket Set Screw - M5x8:4',#19547,#19561,
'Socket Set Screw - M5x8:4');
#222=NEXT_ASSEMBLY_USAGE_OCCURRENCE('Socket Set Screw - M5x8:5',
'Socket Set Screw - M5x8:5','Socket Set Screw - M5x8:5',#19547,#19561,
'Socket Set Screw - M5x8:5');
#223=NEXT_ASSEMBLY_USAGE_OCCURRENCE('Socket Set Screw - M5x8:6',
'Socket Set Screw - M5x8:6','Socket Set Screw - M5x8:6',#19547,#19561,
'Socket Set Screw - M5x8:6');
#224=NEXT_ASSEMBLY_USAGE_OCCURRENCE('Cap Screw - M4x16:2',
'Cap Screw - M4x16:2','Cap Screw - M4x16:2',#19547,#19562,
'Cap Screw - M4x16:2');
#225=NEXT_ASSEMBLY_USAGE_OCCURRENCE('Motor and bearing base:1',
'Motor and bearing base:1','Motor and bearing base:1',#19526,#19527,
'Motor and bearing base:1');
#226=NEXT_ASSEMBLY_USAGE_OCCURRENCE('Coupled rotor:1','Coupled rotor:1',
'Coupled rotor:1',#19526,#19547,'Coupled rotor:1');
#227=B_SPLINE_CURVE_WITH_KNOTS('',3,(#16151,#16152,#16153,#16154,#16155,
#16156,#16157,#16158,#16159,#16160),.UNSPECIFIED.,.F.,.F.,(4,2,2,2,4),(1.13193471301885,
1.22626174930539,1.32058878559194,1.41491753480854,1.50924628402513),
 .UNSPECIFIED.);
#228=B_SPLINE_CURVE_WITH_KNOTS('',3,(#16162,#16163,#16164,#16165,#16166,
#16167,#16168,#16169,#16170,#16171,#16172,#16173,#16174,#16175,#16176,#16177,
#16178,#16179),.UNSPECIFIED.,.F.,.F.,(4,2,2,2,2,2,2,2,4),(0.377311571006283,
0.471638607292829,0.565965643579376,0.66029439279597,0.754623142012565,
0.84895189122916,0.943280640445754,1.0376076767323,1.13193471301885),
 .UNSPECIFIED.);
#229=B_SPLINE_CURVE_WITH_KNOTS('',3,(#16180,#16181,#16182,#16183,#16184,
#16185,#16186,#16187,#16188,#16189),.UNSPECIFIED.,.F.,.F.,(4,2,2,2,4),(1.50924628402513,
1.60357503324173,1.69790378245832,1.79223081874487,1.88655785503141),
 .UNSPECIFIED.);
#230=B_SPLINE_CURVE_WITH_KNOTS('',3,(#16192,#16193,#16194,#16195,#16196,
#16197,#16198,#16199,#16200,#16201,#16202,#16203,#16204,#16205,#16206,#16207,
#16208,#16209,#16210,#16211,#16212,#16213,#16214,#16215,#16216,#16217,#16218,
#16219,#16220,#16221,#16222,#16223,#16224,#16225),.UNSPECIFIED.,.T.,.F.,
(4,2,2,2,2,2,2,2,2,2,2,2,2,2,2,2,4),(0.,0.0955080856649705,0.191016171329941,
0.286408845249646,0.38180151916935,0.477194193089055,0.572586867008759,
0.66809495267373,0.763603038338701,0.859111124003671,0.954619209668642,
1.05001188358835,1.14540455750805,1.24079723142776,1.33618990534746,1.43169799101243,
1.5272060766774),.UNSPECIFIED.);
#231=B_SPLINE_CURVE_WITH_KNOTS('',3,(#16228,#16229,#16230,#16231,#16232,
#16233,#16234,#16235,#16236,#16237,#16238,#16239,#16240,#16241,#16242,#16243,
#16244,#16245,#16246,#16247,#16248,#16249,#16250,#16251,#16252,#16253,#16254,
#16255,#16256,#16257,#16258,#16259,#16260,#16261),.UNSPECIFIED.,.T.,.F.,
(4,2,2,2,2,2,2,2,2,2,2,2,2,2,2,2,4),(0.,0.0955080856649706,0.191016171329941,
0.286408845249646,0.381801519169351,0.477194193089055,0.57258686700876,
0.668094952673731,0.763603038338701,0.859111124003672,0.954619209668642,
1.05001188358835,1.14540455750805,1.24079723142776,1.33618990534746,1.43169799101243,
1.5272060766774),.UNSPECIFIED.);
#232=B_SPLINE_CURVE_WITH_KNOTS('',3,(#16265,#16266,#16267,#16268,#16269,
#16270,#16271,#16272,#16273,#16274),.UNSPECIFIED.,.F.,.F.,(4,2,2,2,4),(1.13193471301885,
1.22626174930539,1.32058878559194,1.41491753480854,1.50924628402513),
 .UNSPECIFIED.);
#233=B_SPLINE_CURVE_WITH_KNOTS('',3,(#16276,#16277,#16278,#16279,#16280,
#16281,#16282,#16283,#16284,#16285,#16286,#16287,#16288,#16289,#16290,#16291,
#16292,#16293),.UNSPECIFIED.,.F.,.F.,(4,2,2,2,2,2,2,2,4),(0.377311571006283,
0.47163860729283,0.565965643579376,0.660294392795971,0.754623142012565,
0.84895189122916,0.943280640445755,1.0376076767323,1.13193471301885),
 .UNSPECIFIED.);
#234=B_SPLINE_CURVE_WITH_KNOTS('',3,(#16294,#16295,#16296,#16297,#16298,
#16299,#16300,#16301,#16302,#16303),.UNSPECIFIED.,.F.,.F.,(4,2,2,2,4),(1.50924628402513,
1.60357503324173,1.69790378245832,1.79223081874487,1.88655785503141),
 .UNSPECIFIED.);
#235=B_SPLINE_CURVE_WITH_KNOTS('',3,(#16312,#16313,#16314,#16315,#16316,
#16317,#16318,#16319,#16320,#16321,#16322,#16323,#16324,#16325,#16326,#16327,
#16328,#16329),.UNSPECIFIED.,.F.,.F.,(4,2,2,2,2,2,2,2,4),(0.377311571006282,
0.471638607292829,0.565965643579376,0.660294392795971,0.754623142012565,
0.84895189122916,0.943280640445754,1.0376076767323,1.13193471301885),
 .UNSPECIFIED.);
#236=B_SPLINE_CURVE_WITH_KNOTS('',3,(#16331,#16332,#16333,#16334,#16335,
#16336,#16337,#16338,#16339,#16340),.UNSPECIFIED.,.F.,.F.,(4,2,2,2,4),(1.13193471301885,
1.22626174930539,1.32058878559194,1.41491753480854,1.50924628402513),
 .UNSPECIFIED.);
#237=B_SPLINE_CURVE_WITH_KNOTS('',3,(#16341,#16342,#16343,#16344,#16345,
#16346,#16347,#16348,#16349,#16350),.UNSPECIFIED.,.F.,.F.,(4,2,2,2,4),(1.50924628402513,
1.60357503324172,1.69790378245832,1.79223081874487,1.88655785503141),
 .UNSPECIFIED.);
#238=B_SPLINE_CURVE_WITH_KNOTS('',3,(#16353,#16354,#16355,#16356,#16357,
#16358,#16359,#16360,#16361,#16362,#16363,#16364,#16365,#16366,#16367,#16368,
#16369,#16370),.UNSPECIFIED.,.F.,.F.,(4,2,2,2,2,2,2,2,4),(0.377311571006283,
0.47163860729283,0.565965643579376,0.660294392795971,0.754623142012565,
0.84895189122916,0.943280640445754,1.0376076767323,1.13193471301885),
 .UNSPECIFIED.);
#239=B_SPLINE_CURVE_WITH_KNOTS('',3,(#16372,#16373,#16374,#16375,#16376,
#16377,#16378,#16379,#16380,#16381),.UNSPECIFIED.,.F.,.F.,(4,2,2,2,4),(1.13193471301885,
1.22626174930539,1.32058878559194,1.41491753480854,1.50924628402513),
 .UNSPECIFIED.);
#240=B_SPLINE_CURVE_WITH_KNOTS('',3,(#16382,#16383,#16384,#16385,#16386,
#16387,#16388,#16389,#16390,#16391),.UNSPECIFIED.,.F.,.F.,(4,2,2,2,4),(1.50924628402513,
1.60357503324173,1.69790378245832,1.79223081874487,1.88655785503141),
 .UNSPECIFIED.);
#241=B_SPLINE_CURVE_WITH_KNOTS('',3,(#16394,#16395,#16396,#16397,#16398,
#16399,#16400,#16401,#16402,#16403,#16404,#16405,#16406,#16407,#16408,#16409,
#16410,#16411),.UNSPECIFIED.,.F.,.F.,(4,2,2,2,2,2,2,2,4),(0.377311571006282,
0.471638607292829,0.565965643579376,0.66029439279597,0.754623142012565,
0.84895189122916,0.943280640445754,1.0376076767323,1.13193471301885),
 .UNSPECIFIED.);
#242=B_SPLINE_CURVE_WITH_KNOTS('',3,(#16413,#16414,#16415,#16416,#16417,
#16418,#16419,#16420,#16421,#16422),.UNSPECIFIED.,.F.,.F.,(4,2,2,2,4),(1.13193471301885,
1.22626174930539,1.32058878559194,1.41491753480854,1.50924628402513),
 .UNSPECIFIED.);
#243=B_SPLINE_CURVE_WITH_KNOTS('',3,(#16423,#16424,#16425,#16426,#16427,
#16428,#16429,#16430,#16431,#16432),.UNSPECIFIED.,.F.,.F.,(4,2,2,2,4),(1.50924628402513,
1.60357503324172,1.69790378245832,1.79223081874487,1.88655785503141),
 .UNSPECIFIED.);
#244=B_SPLINE_CURVE_WITH_KNOTS('',3,(#16435,#16436,#16437,#16438,#16439,
#16440,#16441,#16442,#16443,#16444,#16445,#16446,#16447,#16448,#16449,#16450,
#16451,#16452),.UNSPECIFIED.,.F.,.F.,(4,2,2,2,2,2,2,2,4),(0.377311571006283,
0.471638607292829,0.565965643579376,0.660294392795971,0.754623142012565,
0.84895189122916,0.943280640445755,1.0376076767323,1.13193471301885),
 .UNSPECIFIED.);
#245=B_SPLINE_CURVE_WITH_KNOTS('',3,(#16454,#16455,#16456,#16457,#16458,
#16459,#16460,#16461,#16462,#16463),.UNSPECIFIED.,.F.,.F.,(4,2,2,2,4),(1.13193471301885,
1.22626174930539,1.32058878559194,1.41491753480854,1.50924628402513),
 .UNSPECIFIED.);
#246=B_SPLINE_CURVE_WITH_KNOTS('',3,(#16464,#16465,#16466,#16467,#16468,
#16469,#16470,#16471,#16472,#16473),.UNSPECIFIED.,.F.,.F.,(4,2,2,2,4),(1.50924628402513,
1.60357503324172,1.69790378245832,1.79223081874487,1.88655785503141),
 .UNSPECIFIED.);
#247=B_SPLINE_CURVE_WITH_KNOTS('',3,(#16477,#16478,#16479,#16480,#16481,
#16482,#16483,#16484,#16485,#16486,#16487,#16488,#16489,#16490,#16491,#16492,
#16493,#16494,#16495,#16496,#16497,#16498,#16499,#16500,#16501,#16502,#16503,
#16504,#16505,#16506,#16507,#16508,#16509,#16510),.UNSPECIFIED.,.T.,.F.,
(4,2,2,2,2,2,2,2,2,2,2,2,2,2,2,2,4),(0.,0.0955080856649705,0.191016171329941,
0.286408845249646,0.38180151916935,0.477194193089055,0.572586867008759,
0.66809495267373,0.7636030383387,0.859111124003671,0.954619209668642,1.05001188358835,
1.14540455750805,1.24079723142776,1.33618990534746,1.43169799101243,1.5272060766774),
 .UNSPECIFIED.);
#248=B_SPLINE_CURVE_WITH_KNOTS('',3,(#16513,#16514,#16515,#16516,#16517,
#16518,#16519,#16520,#16521,#16522,#16523,#16524,#16525,#16526,#16527,#16528,
#16529,#16530,#16531,#16532,#16533,#16534,#16535,#16536,#16537,#16538,#16539,
#16540,#16541,#16542,#16543,#16544,#16545,#16546),.UNSPECIFIED.,.T.,.F.,
(4,2,2,2,2,2,2,2,2,2,2,2,2,2,2,2,4),(0.,0.0955080856649706,0.191016171329941,
0.286408845249646,0.381801519169351,0.477194193089055,0.57258686700876,
0.668094952673731,0.763603038338701,0.859111124003672,0.954619209668642,
1.05001188358835,1.14540455750805,1.24079723142776,1.33618990534746,1.43169799101243,
1.5272060766774),.UNSPECIFIED.);
#249=B_SPLINE_CURVE_WITH_KNOTS('',3,(#16551,#16552,#16553,#16554,#16555,
#16556,#16557,#16558,#16559,#16560,#16561,#16562,#16563,#16564,#16565,#16566,
#16567,#16568,#16569,#16570,#16571,#16572,#16573,#16574,#16575,#16576,#16577,
#16578,#16579,#16580,#16581,#16582,#16583,#16584),.UNSPECIFIED.,.T.,.F.,
(4,2,2,2,2,2,2,2,2,2,2,2,2,2,2,2,4),(0.,0.0955080856649705,0.191016171329941,
0.286408845249646,0.38180151916935,0.477194193089055,0.572586867008759,
0.66809495267373,0.7636030383387,0.859111124003671,0.954619209668642,1.05001188358835,
1.14540455750805,1.24079723142776,1.33618990534746,1.43169799101243,1.5272060766774),
 .UNSPECIFIED.);
#250=B_SPLINE_CURVE_WITH_KNOTS('',3,(#16587,#16588,#16589,#16590,#16591,
#16592,#16593,#16594,#16595,#16596,#16597,#16598,#16599,#16600,#16601,#16602,
#16603,#16604,#16605,#16606,#16607,#16608,#16609,#16610,#16611,#16612,#16613,
#16614,#16615,#16616,#16617,#16618,#16619,#16620),.UNSPECIFIED.,.T.,.F.,
(4,2,2,2,2,2,2,2,2,2,2,2,2,2,2,2,4),(0.,0.0955080856649706,0.191016171329941,
0.286408845249646,0.381801519169351,0.477194193089055,0.57258686700876,
0.668094952673731,0.763603038338701,0.859111124003672,0.954619209668642,
1.05001188358835,1.14540455750805,1.24079723142776,1.33618990534746,1.43169799101243,
1.5272060766774),.UNSPECIFIED.);
#251=B_SPLINE_CURVE_WITH_KNOTS('',3,(#16870,#16871,#16872,#16873,#16874,
#16875,#16876,#16877,#16878,#16879),.UNSPECIFIED.,.F.,.F.,(4,2,2,2,4),(0.705412572778712,
0.711709336094043,0.776040013313971,0.840370690533898,0.846667453849229),
 .UNSPECIFIED.);
#252=B_SPLINE_CURVE_WITH_KNOTS('',3,(#16885,#16886,#16887,#16888,#16889,
#16890,#16891,#16892,#16893,#16894,#16895,#16896,#16897,#16898,#16899,#16900,
#16901,#16902),.UNSPECIFIED.,.F.,.F.,(4,2,2,2,2,2,2,2,4),(0.,0.0625085224334669,
0.125017044866934,0.187512605393579,0.250008165920225,0.312503726446871,
0.374999286973516,0.437507809406983,0.50001633184045),.UNSPECIFIED.);
#253=B_SPLINE_CURVE_WITH_KNOTS('',3,(#16903,#16904,#16905,#16906,#16907,
#16908,#16909,#16910,#16911,#16912,#16913,#16914,#16915,#16916,#16917,#16918,
#16919,#16920),.UNSPECIFIED.,.F.,.F.,(4,2,2,2,2,2,2,2,4),(0.50001633184045,
0.562524854273917,0.625033376707384,0.687528937234029,0.750024497760675,
0.81252005828732,0.875015618813966,0.937524141247433,1.0000326636809),
 .UNSPECIFIED.);
#254=B_SPLINE_CURVE_WITH_KNOTS('',3,(#16923,#16924,#16925,#16926,#16927,
#16928,#16929,#16930,#16931,#16932),.UNSPECIFIED.,.F.,.F.,(4,2,2,2,4),(0.188052563902732,
0.194349327218063,0.25868000443799,0.323010681657918,0.329307444973249),
 .UNSPECIFIED.);
#255=B_SPLINE_CURVE_WITH_KNOTS('',3,(#16957,#16958,#16959,#16960,#16961,
#16962,#16963,#16964,#16965,#16966),.UNSPECIFIED.,.F.,.F.,(4,2,2,2,4),(0.847831445683403,
0.87827457693095,0.958092875386316,1.03791117384168,1.06835430508923),
 .UNSPECIFIED.);
#256=B_SPLINE_CURVE_WITH_KNOTS('',3,(#16972,#16973,#16974,#16975,#16976,
#16977,#16978,#16979,#16980,#16981,#16982,#16983,#16984,#16985,#16986,#16987,
#16988,#16989),.UNSPECIFIED.,.F.,.F.,(4,2,2,2,2,2,2,2,4),(0.,0.0792812130427884,
0.158562426085577,0.237841058284634,0.317119690483692,0.396398322682749,
0.475676954881807,0.554958167924595,0.634239380967384),.UNSPECIFIED.);
#257=B_SPLINE_CURVE_WITH_KNOTS('',3,(#16990,#16991,#16992,#16993,#16994,
#16995,#16996,#16997,#16998,#16999,#17000,#17001,#17002,#17003,#17004,#17005,
#17006,#17007),.UNSPECIFIED.,.F.,.F.,(4,2,2,2,2,2,2,2,4),(0.634239380967384,
0.713520594010172,0.792801807052961,0.872080439252018,0.951359071451076,
1.03063770365013,1.10991633584919,1.18919754889198,1.26847876193477),
 .UNSPECIFIED.);
#258=B_SPLINE_CURVE_WITH_KNOTS('',3,(#17010,#17011,#17012,#17013,#17014,
#17015,#17016,#17017,#17018,#17019),.UNSPECIFIED.,.F.,.F.,(4,2,2,2,4),(0.209102862092526,
0.239545993340073,0.319364291795439,0.399182590250804,0.429625721498351),
 .UNSPECIFIED.);
#259=B_SPLINE_CURVE_WITH_KNOTS('',3,(#17076,#17077,#17078,#17079,#17080,
#17081,#17082,#17083,#17084,#17085),.UNSPECIFIED.,.F.,.F.,(4,2,2,2,4),(0.818088904349167,
0.878131747417164,0.957937926194035,1.03774410497091,1.0977869480389),
 .UNSPECIFIED.);
#260=B_SPLINE_CURVE_WITH_KNOTS('',3,(#17091,#17092,#17093,#17094,#17095,
#17096,#17097,#17098,#17099,#17100,#17101,#17102,#17103,#17104,#17105,#17106,
#17107,#17108),.UNSPECIFIED.,.F.,.F.,(4,2,2,2,2,2,2,2,4),(0.,0.0793157643915217,
0.158631528783043,0.237943615933649,0.317255703084255,0.396567790234861,
0.475879877385467,0.555195641776989,0.63451140616851),.UNSPECIFIED.);
#261=B_SPLINE_CURVE_WITH_KNOTS('',3,(#17109,#17110,#17111,#17112,#17113,
#17114,#17115,#17116,#17117,#17118,#17119,#17120,#17121,#17122,#17123,#17124,
#17125,#17126),.UNSPECIFIED.,.F.,.F.,(4,2,2,2,2,2,2,2,4),(0.63451140616851,
0.713827170560032,0.793142934951554,0.87245502210216,0.951767109252766,
1.03107919640337,1.11039128355398,1.1897070479455,1.26902281233702),
 .UNSPECIFIED.);
#262=B_SPLINE_CURVE_WITH_KNOTS('',3,(#17129,#17130,#17131,#17132,#17133,
#17134,#17135,#17136,#17137,#17138),.UNSPECIFIED.,.F.,.F.,(4,2,2,2,4),(0.179463620219811,
0.239506463287807,0.319312642064678,0.399118820841549,0.459161663909546),
 .UNSPECIFIED.);
#263=B_SPLINE_CURVE_WITH_KNOTS('',3,(#17163,#17164,#17165,#17166,#17167,
#17168,#17169,#17170,#17171,#17172),.UNSPECIFIED.,.F.,.F.,(4,2,2,2,4),(0.818088904349168,
0.878131747417163,0.957937926194034,1.03774410497091,1.0977869480389),
 .UNSPECIFIED.);
#264=B_SPLINE_CURVE_WITH_KNOTS('',3,(#17178,#17179,#17180,#17181,#17182,
#17183,#17184,#17185,#17186,#17187,#17188,#17189,#17190,#17191,#17192,#17193,
#17194,#17195),.UNSPECIFIED.,.F.,.F.,(4,2,2,2,2,2,2,2,4),(0.,0.079315764391521,
0.158631528783042,0.237943615933648,0.317255703084255,0.396567790234861,
0.475879877385467,0.555195641776988,0.634511406168509),.UNSPECIFIED.);
#265=B_SPLINE_CURVE_WITH_KNOTS('',3,(#17196,#17197,#17198,#17199,#17200,
#17201,#17202,#17203,#17204,#17205,#17206,#17207,#17208,#17209,#17210,#17211,
#17212,#17213),.UNSPECIFIED.,.F.,.F.,(4,2,2,2,2,2,2,2,4),(0.634511406168509,
0.71382717056003,0.793142934951551,0.872455022102158,0.951767109252764,
1.03107919640337,1.11039128355398,1.1897070479455,1.26902281233702),
 .UNSPECIFIED.);
#266=B_SPLINE_CURVE_WITH_KNOTS('',3,(#17216,#17217,#17218,#17219,#17220,
#17221,#17222,#17223,#17224,#17225),.UNSPECIFIED.,.F.,.F.,(4,2,2,2,4),(0.179463620219808,
0.239506463287807,0.319312642064678,0.399118820841549,0.459161663909549),
 .UNSPECIFIED.);
#267=B_SPLINE_CURVE_WITH_KNOTS('',3,(#17316,#17317,#17318,#17319,#17320,
#17321,#17322,#17323,#17324,#17325,#17326,#17327,#17328,#17329,#17330,#17331,
#17332,#17333),.UNSPECIFIED.,.F.,.F.,(4,2,2,2,2,2,2,2,4),(0.,0.0798638474423531,
0.159727694884706,0.239545993340072,0.319364291795438,0.399182590250804,
0.47900088870617,0.558864736148523,0.638728583590876),.UNSPECIFIED.);
#268=B_SPLINE_CURVE_WITH_KNOTS('',3,(#17334,#17335,#17336,#17337,#17338,
#17339,#17340,#17341,#17342,#17343,#17344,#17345,#17346,#17347,#17348,#17349,
#17350,#17351),.UNSPECIFIED.,.F.,.F.,(4,2,2,2,2,2,2,2,4),(0.638728583590876,
0.718592431033229,0.798456278475582,0.878274576930948,0.958092875386314,
1.03791117384168,1.11772947229705,1.1975933197394,1.27745716718175),
 .UNSPECIFIED.);
#269=B_SPLINE_CURVE_WITH_KNOTS('',3,(#17354,#17355,#17356,#17357,#17358,
#17359,#17360,#17361,#17362,#17363,#17364,#17365,#17366,#17367,#17368,#17369,
#17370,#17371,#17372,#17373,#17374,#17375,#17376,#17377,#17378,#17379,#17380,
#17381,#17382,#17383,#17384,#17385,#17386,#17387),.UNSPECIFIED.,.T.,.F.,
(4,2,2,2,2,2,2,2,2,2,2,2,2,2,2,2,4),(0.,0.079239302416133,0.158478604832266,
0.237716399152057,0.316954193471848,0.39619198779164,0.475429782111431,
0.554669084527564,0.633908386943697,0.71314768935983,0.792386991775963,
0.871624786095754,0.950862580415545,1.03010037473534,1.10933816905513,1.18857747147126,
1.26781677388739),.UNSPECIFIED.);
#270=B_SPLINE_CURVE_WITH_KNOTS('',3,(#17784,#17785,#17786,#17787,#17788,
#17789,#17790,#17791,#17792,#17793,#17794,#17795,#17796,#17797,#17798,#17799,
#17800,#17801),.UNSPECIFIED.,.F.,.F.,(4,2,2,2,2,2,2,2,4),(0.,0.0798638474423531,
0.159727694884706,0.239545993340072,0.319364291795438,0.399182590250804,
0.47900088870617,0.558864736148523,0.638728583590876),.UNSPECIFIED.);
#271=B_SPLINE_CURVE_WITH_KNOTS('',3,(#17802,#17803,#17804,#17805,#17806,
#17807,#17808,#17809,#17810,#17811,#17812,#17813,#17814,#17815,#17816,#17817,
#17818,#17819),.UNSPECIFIED.,.F.,.F.,(4,2,2,2,2,2,2,2,4),(0.638728583590876,
0.718592431033229,0.798456278475583,0.878274576930949,0.958092875386314,
1.03791117384168,1.11772947229705,1.1975933197394,1.27745716718175),
 .UNSPECIFIED.);
#272=B_SPLINE_CURVE_WITH_KNOTS('',3,(#17823,#17824,#17825,#17826,#17827,
#17828,#17829,#17830,#17831,#17832,#17833,#17834,#17835,#17836,#17837,#17838,
#17839,#17840),.UNSPECIFIED.,.F.,.F.,(4,2,2,2,2,2,2,2,4),(0.,0.079239302416133,
0.158478604832266,0.237716399152057,0.316954193471848,0.39619198779164,
0.475429782111431,0.554669084527564,0.633908386943697),.UNSPECIFIED.);
#273=B_SPLINE_CURVE_WITH_KNOTS('',3,(#17841,#17842,#17843,#17844,#17845,
#17846,#17847,#17848,#17849,#17850,#17851,#17852,#17853,#17854,#17855,#17856,
#17857,#17858),.UNSPECIFIED.,.F.,.F.,(4,2,2,2,2,2,2,2,4),(0.633908386943697,
0.71314768935983,0.792386991775963,0.871624786095754,0.950862580415545,
1.03010037473534,1.10933816905513,1.18857747147126,1.26781677388739),
 .UNSPECIFIED.);
#274=SPHERICAL_SURFACE('',#11594,2.35);
#275=SPHERICAL_SURFACE('',#11636,2.35);
#276=SHAPE_REPRESENTATION_RELATIONSHIP('SRR','None',#19490,#308);
#277=SHAPE_REPRESENTATION_RELATIONSHIP('SRR','None',#19491,#309);
#278=SHAPE_REPRESENTATION_RELATIONSHIP('SRR','None',#19492,#310);
#279=SHAPE_REPRESENTATION_RELATIONSHIP('SRR','None',#19493,#311);
#280=SHAPE_REPRESENTATION_RELATIONSHIP('SRR','None',#19494,#312);
#281=SHAPE_REPRESENTATION_RELATIONSHIP('SRR','None',#19495,#313);
#282=SHAPE_REPRESENTATION_RELATIONSHIP('SRR','None',#19496,#314);
#283=SHAPE_REPRESENTATION_RELATIONSHIP('SRR','None',#19497,#315);
#284=SHAPE_REPRESENTATION_RELATIONSHIP('SRR','None',#19498,#316);
#285=SHAPE_REPRESENTATION_RELATIONSHIP('SRR','None',#19499,#317);
#286=SHAPE_REPRESENTATION_RELATIONSHIP('SRR','None',#19500,#318);
#287=SHAPE_REPRESENTATION_RELATIONSHIP('SRR','None',#19501,#319);
#288=SHAPE_REPRESENTATION_RELATIONSHIP('SRR','None',#19502,#320);
#289=SHAPE_REPRESENTATION_RELATIONSHIP('SRR','None',#19504,#321);
#290=SHAPE_REPRESENTATION_RELATIONSHIP('SRR','None',#19505,#322);
#291=SHAPE_REPRESENTATION_RELATIONSHIP('SRR','None',#19506,#323);
#292=SHAPE_REPRESENTATION_RELATIONSHIP('SRR','None',#19507,#324);
#293=SHAPE_REPRESENTATION_RELATIONSHIP('SRR','None',#19508,#325);
#294=SHAPE_REPRESENTATION_RELATIONSHIP('SRR','None',#19510,#326);
#295=SHAPE_REPRESENTATION_RELATIONSHIP('SRR','None',#19511,#327);
#296=SHAPE_REPRESENTATION_RELATIONSHIP('SRR','None',#19512,#328);
#297=SHAPE_REPRESENTATION_RELATIONSHIP('SRR','None',#19513,#329);
#298=SHAPE_REPRESENTATION_RELATIONSHIP('SRR','None',#19514,#330);
#299=SHAPE_REPRESENTATION_RELATIONSHIP('SRR','None',#19515,#331);
#300=SHAPE_REPRESENTATION_RELATIONSHIP('SRR','None',#19516,#332);
#301=SHAPE_REPRESENTATION_RELATIONSHIP('SRR','None',#19517,#333);
#302=SHAPE_REPRESENTATION_RELATIONSHIP('SRR','None',#19519,#334);
#303=SHAPE_REPRESENTATION_RELATIONSHIP('SRR','None',#19520,#335);
#304=SHAPE_REPRESENTATION_RELATIONSHIP('SRR','None',#19521,#336);
#305=SHAPE_REPRESENTATION_RELATIONSHIP('SRR','None',#19522,#337);
#306=SHAPE_REPRESENTATION_RELATIONSHIP('SRR','None',#19523,#338);
#307=SHAPE_REPRESENTATION_RELATIONSHIP('SRR','None',#19524,#339);
#308=ADVANCED_BREP_SHAPE_REPRESENTATION('',(#373),#19326);
#309=ADVANCED_BREP_SHAPE_REPRESENTATION('',(#374),#19327);
#310=ADVANCED_BREP_SHAPE_REPRESENTATION('',(#375),#19328);
#311=ADVANCED_BREP_SHAPE_REPRESENTATION('',(#376),#19329);
#312=ADVANCED_BREP_SHAPE_REPRESENTATION('',(#377),#19330);
#313=ADVANCED_BREP_SHAPE_REPRESENTATION('',(#378),#19331);
#314=ADVANCED_BREP_SHAPE_REPRESENTATION('',(#379),#19332);
#315=ADVANCED_BREP_SHAPE_REPRESENTATION('',(#380),#19333);
#316=ADVANCED_BREP_SHAPE_REPRESENTATION('',(#381),#19334);
#317=ADVANCED_BREP_SHAPE_REPRESENTATION('',(#382),#19335);
#318=ADVANCED_BREP_SHAPE_REPRESENTATION('',(#383),#19336);
#319=ADVANCED_BREP_SHAPE_REPRESENTATION('',(#384),#19337);
#320=ADVANCED_BREP_SHAPE_REPRESENTATION('',(#385),#19338);
#321=ADVANCED_BREP_SHAPE_REPRESENTATION('',(#386),#19340);
#322=ADVANCED_BREP_SHAPE_REPRESENTATION('',(#387,#388),#19341);
#323=ADVANCED_BREP_SHAPE_REPRESENTATION('',(#389),#19342);
#324=ADVANCED_BREP_SHAPE_REPRESENTATION('',(#32),#19343);
#325=ADVANCED_BREP_SHAPE_REPRESENTATION('',(#33),#19344);
#326=ADVANCED_BREP_SHAPE_REPRESENTATION('',(#390),#19346);
#327=ADVANCED_BREP_SHAPE_REPRESENTATION('',(#391),#19347);
#328=ADVANCED_BREP_SHAPE_REPRESENTATION('',(#392),#19348);
#329=ADVANCED_BREP_SHAPE_REPRESENTATION('',(#393),#19349);
#330=ADVANCED_BREP_SHAPE_REPRESENTATION('',(#394),#19350);
#331=ADVANCED_BREP_SHAPE_REPRESENTATION('',(#395),#19351);
#332=ADVANCED_BREP_SHAPE_REPRESENTATION('',(#396),#19352);
#333=ADVANCED_BREP_SHAPE_REPRESENTATION('',(#397),#19353);
#334=ADVANCED_BREP_SHAPE_REPRESENTATION('',(#398),#19355);
#335=ADVANCED_BREP_SHAPE_REPRESENTATION('',(#399),#19356);
#336=ADVANCED_BREP_SHAPE_REPRESENTATION('',(#400),#19357);
#337=ADVANCED_BREP_SHAPE_REPRESENTATION('',(#401),#19358);
#338=ADVANCED_BREP_SHAPE_REPRESENTATION('',(#402),#19359);
#339=ADVANCED_BREP_SHAPE_REPRESENTATION('',(#34),#19360);
#340=STYLED_ITEM('',(#19725),#373);
#341=STYLED_ITEM('',(#19760),#374);
#342=STYLED_ITEM('',(#19760),#375);
#343=STYLED_ITEM('',(#19739),#376);
#344=STYLED_ITEM('',(#19739),#377);
#345=STYLED_ITEM('',(#19739),#378);
#346=STYLED_ITEM('',(#19739),#379);
#347=STYLED_ITEM('',(#19725),#380);
#348=STYLED_ITEM('',(#19739),#381);
#349=STYLED_ITEM('',(#19753),#382);
#350=STYLED_ITEM('',(#19753),#383);
#351=STYLED_ITEM('',(#19753),#384);
#352=STYLED_ITEM('',(#19753),#385);
#353=STYLED_ITEM('',(#19725),#386);
#354=STYLED_ITEM('',(#19746),#387);
#355=STYLED_ITEM('',(#19746),#388);
#356=STYLED_ITEM('',(#19753),#389);
#357=STYLED_ITEM('',(#19753),#32);
#358=STYLED_ITEM('',(#19753),#33);
#359=STYLED_ITEM('',(#19746),#390);
#360=STYLED_ITEM('',(#19746),#391);
#361=STYLED_ITEM('',(#19746),#392);
#362=STYLED_ITEM('',(#19760),#393);
#363=STYLED_ITEM('',(#19746),#394);
#364=STYLED_ITEM('',(#19746),#395);
#365=STYLED_ITEM('',(#19746),#396);
#366=STYLED_ITEM('',(#19753),#397);
#367=STYLED_ITEM('',(#19739),#398);
#368=STYLED_ITEM('',(#19739),#399);
#369=STYLED_ITEM('',(#19739),#400);
#370=STYLED_ITEM('',(#19746),#401);
#371=STYLED_ITEM('',(#19753),#402);
#372=STYLED_ITEM('',(#19753),#34);
#373=MANIFOLD_SOLID_BREP('Body1',#10984);
#374=MANIFOLD_SOLID_BREP('Body1',#10985);
#375=MANIFOLD_SOLID_BREP('Body1',#10986);
#376=MANIFOLD_SOLID_BREP('Body1',#10987);
#377=MANIFOLD_SOLID_BREP('Body1',#10988);
#378=MANIFOLD_SOLID_BREP('Body1',#10989);
#379=MANIFOLD_SOLID_BREP('Body1',#10990);
#380=MANIFOLD_SOLID_BREP('Body1',#10991);
#381=MANIFOLD_SOLID_BREP('Body1',#10992);
#382=MANIFOLD_SOLID_BREP('Body1',#10993);
#383=MANIFOLD_SOLID_BREP('Body1',#10994);
#384=MANIFOLD_SOLID_BREP('Body1',#10995);
#385=MANIFOLD_SOLID_BREP('Body1',#10996);
#386=MANIFOLD_SOLID_BREP('Body1',#10997);
#387=MANIFOLD_SOLID_BREP('Body1',#10998);
#388=MANIFOLD_SOLID_BREP('Body2',#10999);
#389=MANIFOLD_SOLID_BREP('Body1',#11000);
#390=MANIFOLD_SOLID_BREP('Body1',#11005);
#391=MANIFOLD_SOLID_BREP('Body1',#11006);
#392=MANIFOLD_SOLID_BREP('Body1',#11007);
#393=MANIFOLD_SOLID_BREP('Body1',#11008);
#394=MANIFOLD_SOLID_BREP('Body1',#11009);
#395=MANIFOLD_SOLID_BREP('Body1',#11010);
#396=MANIFOLD_SOLID_BREP('Body1',#11011);
#397=MANIFOLD_SOLID_BREP('Body1',#11012);
#398=MANIFOLD_SOLID_BREP('Body1',#11013);
#399=MANIFOLD_SOLID_BREP('Body1',#11014);
#400=MANIFOLD_SOLID_BREP('Body1',#11015);
#401=MANIFOLD_SOLID_BREP('Body1',#11016);
#402=MANIFOLD_SOLID_BREP('Body1',#11017);
#403=FACE_BOUND('',#1653,.T.);
#404=FACE_BOUND('',#1654,.T.);
#405=FACE_BOUND('',#1655,.T.);
#406=FACE_BOUND('',#1656,.T.);
#407=FACE_BOUND('',#1657,.T.);
#408=FACE_BOUND('',#1658,.T.);
#409=FACE_BOUND('',#1660,.T.);
#410=FACE_BOUND('',#1661,.T.);
#411=FACE_BOUND('',#1662,.T.);
#412=FACE_BOUND('',#1663,.T.);
#413=FACE_BOUND('',#1664,.T.);
#414=FACE_BOUND('',#1665,.T.);
#415=FACE_BOUND('',#1681,.T.);
#416=FACE_BOUND('',#1683,.T.);
#417=FACE_BOUND('',#1687,.T.);
#418=FACE_BOUND('',#1689,.T.);
#419=FACE_BOUND('',#1693,.T.);
#420=FACE_BOUND('',#1695,.T.);
#421=FACE_BOUND('',#1699,.T.);
#422=FACE_BOUND('',#1701,.T.);
#423=FACE_BOUND('',#1710,.T.);
#424=FACE_BOUND('',#1711,.T.);
#425=FACE_BOUND('',#1714,.T.);
#426=FACE_BOUND('',#1715,.T.);
#427=FACE_BOUND('',#1716,.T.);
#428=FACE_BOUND('',#1717,.T.);
#429=FACE_BOUND('',#1718,.T.);
#430=FACE_BOUND('',#1722,.T.);
#431=FACE_BOUND('',#1723,.T.);
#432=FACE_BOUND('',#1724,.T.);
#433=FACE_BOUND('',#1725,.T.);
#434=FACE_BOUND('',#1726,.T.);
#435=FACE_BOUND('',#1729,.T.);
#436=FACE_BOUND('',#1730,.T.);
#437=FACE_BOUND('',#1741,.T.);
#438=FACE_BOUND('',#1744,.T.);
#439=FACE_BOUND('',#1745,.T.);
#440=FACE_BOUND('',#1746,.T.);
#441=FACE_BOUND('',#1747,.T.);
#442=FACE_BOUND('',#1748,.T.);
#443=FACE_BOUND('',#1751,.T.);
#444=FACE_BOUND('',#1763,.T.);
#445=FACE_BOUND('',#1766,.T.);
#446=FACE_BOUND('',#1777,.T.);
#447=FACE_BOUND('',#1780,.T.);
#448=FACE_BOUND('',#1791,.T.);
#449=FACE_BOUND('',#1794,.T.);
#450=FACE_BOUND('',#1805,.T.);
#451=FACE_BOUND('',#1808,.T.);
#452=FACE_BOUND('',#1817,.T.);
#453=FACE_BOUND('',#1818,.T.);
#454=FACE_BOUND('',#1826,.T.);
#455=FACE_BOUND('',#1827,.T.);
#456=FACE_BOUND('',#1828,.T.);
#457=FACE_BOUND('',#1845,.T.);
#458=FACE_BOUND('',#1846,.T.);
#459=FACE_BOUND('',#1847,.T.);
#460=FACE_BOUND('',#1850,.T.);
#461=FACE_BOUND('',#1852,.T.);
#462=FACE_BOUND('',#1853,.T.);
#463=FACE_BOUND('',#1855,.T.);
#464=FACE_BOUND('',#1859,.T.);
#465=FACE_BOUND('',#1860,.T.);
#466=FACE_BOUND('',#1861,.T.);
#467=FACE_BOUND('',#1862,.T.);
#468=FACE_BOUND('',#1863,.T.);
#469=FACE_BOUND('',#1864,.T.);
#470=FACE_BOUND('',#1870,.T.);
#471=FACE_BOUND('',#1872,.T.);
#472=FACE_BOUND('',#1875,.T.);
#473=FACE_BOUND('',#1877,.T.);
#474=FACE_BOUND('',#1878,.T.);
#475=FACE_BOUND('',#1879,.T.);
#476=FACE_BOUND('',#1880,.T.);
#477=FACE_BOUND('',#1881,.T.);
#478=FACE_BOUND('',#1882,.T.);
#479=FACE_BOUND('',#1886,.T.);
#480=FACE_BOUND('',#1888,.T.);
#481=FACE_BOUND('',#1903,.T.);
#482=FACE_BOUND('',#1920,.T.);
#483=FACE_BOUND('',#1931,.T.);
#484=FACE_BOUND('',#1933,.T.);
#485=FACE_BOUND('',#1942,.T.);
#486=FACE_BOUND('',#1944,.T.);
#487=FACE_BOUND('',#1946,.T.);
#488=FACE_BOUND('',#1948,.T.);
#489=FACE_BOUND('',#1956,.T.);
#490=FACE_BOUND('',#1958,.T.);
#491=FACE_BOUND('',#1960,.T.);
#492=FACE_BOUND('',#1962,.T.);
#493=FACE_BOUND('',#1965,.T.);
#494=FACE_BOUND('',#1968,.T.);
#495=FACE_BOUND('',#1973,.T.);
#496=FACE_BOUND('',#1975,.T.);
#497=FACE_BOUND('',#1977,.T.);
#498=FACE_BOUND('',#1979,.T.);
#499=FACE_BOUND('',#1984,.T.);
#500=FACE_BOUND('',#1986,.T.);
#501=FACE_BOUND('',#1988,.T.);
#502=FACE_BOUND('',#1990,.T.);
#503=FACE_BOUND('',#1994,.T.);
#504=FACE_BOUND('',#1996,.T.);
#505=FACE_BOUND('',#2005,.T.);
#506=FACE_BOUND('',#2012,.T.);
#507=FACE_BOUND('',#2041,.T.);
#508=FACE_BOUND('',#2097,.T.);
#509=FACE_BOUND('',#2099,.T.);
#510=FACE_BOUND('',#2102,.T.);
#511=FACE_BOUND('',#2129,.T.);
#512=FACE_BOUND('',#2187,.T.);
#513=FACE_BOUND('',#2189,.T.);
#514=FACE_BOUND('',#2352,.T.);
#515=FACE_BOUND('',#2362,.T.);
#516=PLANE('',#11394);
#517=PLANE('',#11395);
#518=PLANE('',#11396);
#519=PLANE('',#11397);
#520=PLANE('',#11398);
#521=PLANE('',#11399);
#522=PLANE('',#11401);
#523=PLANE('',#11402);
#524=PLANE('',#11403);
#525=PLANE('',#11404);
#526=PLANE('',#11405);
#527=PLANE('',#11406);
#528=PLANE('',#11408);
#529=PLANE('',#11409);
#530=PLANE('',#11410);
#531=PLANE('',#11411);
#532=PLANE('',#11412);
#533=PLANE('',#11413);
#534=PLANE('',#11421);
#535=PLANE('',#11422);
#536=PLANE('',#11430);
#537=PLANE('',#11431);
#538=PLANE('',#11439);
#539=PLANE('',#11440);
#540=PLANE('',#11448);
#541=PLANE('',#11449);
#542=PLANE('',#11472);
#543=PLANE('',#11473);
#544=PLANE('',#11474);
#545=PLANE('',#11475);
#546=PLANE('',#11476);
#547=PLANE('',#11477);
#548=PLANE('',#11478);
#549=PLANE('',#11479);
#550=PLANE('',#11484);
#551=PLANE('',#11488);
#552=PLANE('',#11492);
#553=PLANE('',#11496);
#554=PLANE('',#11500);
#555=PLANE('',#11504);
#556=PLANE('',#11505);
#557=PLANE('',#11506);
#558=PLANE('',#11507);
#559=PLANE('',#11508);
#560=PLANE('',#11509);
#561=PLANE('',#11511);
#562=PLANE('',#11512);
#563=PLANE('',#11513);
#564=PLANE('',#11514);
#565=PLANE('',#11515);
#566=PLANE('',#11516);
#567=PLANE('',#11517);
#568=PLANE('',#11518);
#569=PLANE('',#11523);
#570=PLANE('',#11526);
#571=PLANE('',#11528);
#572=PLANE('',#11529);
#573=PLANE('',#11530);
#574=PLANE('',#11531);
#575=PLANE('',#11532);
#576=PLANE('',#11533);
#577=PLANE('',#11534);
#578=PLANE('',#11535);
#579=PLANE('',#11540);
#580=PLANE('',#11543);
#581=PLANE('',#11545);
#582=PLANE('',#11546);
#583=PLANE('',#11547);
#584=PLANE('',#11548);
#585=PLANE('',#11549);
#586=PLANE('',#11550);
#587=PLANE('',#11551);
#588=PLANE('',#11552);
#589=PLANE('',#11557);
#590=PLANE('',#11560);
#591=PLANE('',#11562);
#592=PLANE('',#11563);
#593=PLANE('',#11564);
#594=PLANE('',#11565);
#595=PLANE('',#11566);
#596=PLANE('',#11567);
#597=PLANE('',#11568);
#598=PLANE('',#11569);
#599=PLANE('',#11574);
#600=PLANE('',#11577);
#601=PLANE('',#11580);
#602=PLANE('',#11591);
#603=PLANE('',#11592);
#604=PLANE('',#11596);
#605=PLANE('',#11598);
#606=PLANE('',#11600);
#607=PLANE('',#11602);
#608=PLANE('',#11603);
#609=PLANE('',#11605);
#610=PLANE('',#11606);
#611=PLANE('',#11614);
#612=PLANE('',#11615);
#613=PLANE('',#11616);
#614=PLANE('',#11617);
#615=PLANE('',#11618);
#616=PLANE('',#11619);
#617=PLANE('',#11620);
#618=PLANE('',#11625);
#619=PLANE('',#11626);
#620=PLANE('',#11627);
#621=PLANE('',#11628);
#622=PLANE('',#11629);
#623=PLANE('',#11634);
#624=PLANE('',#11639);
#625=PLANE('',#11649);
#626=PLANE('',#11651);
#627=PLANE('',#11655);
#628=PLANE('',#11667);
#629=PLANE('',#11668);
#630=PLANE('',#11670);
#631=PLANE('',#11671);
#632=PLANE('',#11672);
#633=PLANE('',#11673);
#634=PLANE('',#11674);
#635=PLANE('',#11675);
#636=PLANE('',#11676);
#637=PLANE('',#11677);
#638=PLANE('',#11678);
#639=PLANE('',#11680);
#640=PLANE('',#11688);
#641=PLANE('',#11694);
#642=PLANE('',#11695);
#643=PLANE('',#11696);
#644=PLANE('',#11697);
#645=PLANE('',#11698);
#646=PLANE('',#11699);
#647=PLANE('',#11700);
#648=PLANE('',#11701);
#649=PLANE('',#11702);
#650=PLANE('',#11704);
#651=PLANE('',#11712);
#652=PLANE('',#11744);
#653=PLANE('',#11745);
#654=PLANE('',#11747);
#655=PLANE('',#11748);
#656=PLANE('',#11749);
#657=PLANE('',#11754);
#658=PLANE('',#11758);
#659=PLANE('',#11759);
#660=PLANE('',#11764);
#661=PLANE('',#11765);
#662=PLANE('',#11767);
#663=PLANE('',#11772);
#664=PLANE('',#11779);
#665=PLANE('',#11780);
#666=PLANE('',#11782);
#667=PLANE('',#11787);
#668=PLANE('',#11788);
#669=PLANE('',#11789);
#670=PLANE('',#11790);
#671=PLANE('',#11791);
#672=PLANE('',#11796);
#673=PLANE('',#11799);
#674=PLANE('',#11806);
#675=PLANE('',#11808);
#676=PLANE('',#11813);
#677=PLANE('',#11820);
#678=PLANE('',#11821);
#679=PLANE('',#11823);
#680=PLANE('',#11828);
#681=PLANE('',#11835);
#682=PLANE('',#11836);
#683=PLANE('',#11844);
#684=PLANE('',#11845);
#685=PLANE('',#11847);
#686=PLANE('',#11848);
#687=PLANE('',#11849);
#688=PLANE('',#11850);
#689=PLANE('',#11851);
#690=PLANE('',#11852);
#691=PLANE('',#11853);
#692=PLANE('',#11854);
#693=PLANE('',#11862);
#694=PLANE('',#11869);
#695=PLANE('',#11870);
#696=PLANE('',#11871);
#697=PLANE('',#11872);
#698=PLANE('',#11873);
#699=PLANE('',#11874);
#700=PLANE('',#11875);
#701=PLANE('',#11876);
#702=PLANE('',#11877);
#703=PLANE('',#11878);
#704=PLANE('',#11879);
#705=PLANE('',#11880);
#706=PLANE('',#11881);
#707=PLANE('',#11882);
#708=PLANE('',#11883);
#709=PLANE('',#11884);
#710=PLANE('',#11885);
#711=PLANE('',#11886);
#712=PLANE('',#11887);
#713=PLANE('',#11888);
#714=PLANE('',#11890);
#715=PLANE('',#11892);
#716=PLANE('',#11894);
#717=PLANE('',#11896);
#718=PLANE('',#11898);
#719=PLANE('',#11900);
#720=PLANE('',#11902);
#721=PLANE('',#11904);
#722=PLANE('',#11909);
#723=PLANE('',#11910);
#724=PLANE('',#11911);
#725=PLANE('',#11912);
#726=PLANE('',#11913);
#727=PLANE('',#11914);
#728=PLANE('',#11915);
#729=PLANE('',#11916);
#730=PLANE('',#11917);
#731=PLANE('',#11918);
#732=PLANE('',#11919);
#733=PLANE('',#11920);
#734=PLANE('',#11921);
#735=PLANE('',#11922);
#736=PLANE('',#11923);
#737=PLANE('',#11924);
#738=PLANE('',#11925);
#739=PLANE('',#11926);
#740=PLANE('',#11927);
#741=PLANE('',#11928);
#742=PLANE('',#11930);
#743=PLANE('',#11932);
#744=PLANE('',#11934);
#745=PLANE('',#11936);
#746=PLANE('',#11938);
#747=PLANE('',#11940);
#748=PLANE('',#11942);
#749=PLANE('',#11944);
#750=PLANE('',#11945);
#751=PLANE('',#11946);
#752=PLANE('',#11947);
#753=PLANE('',#11948);
#754=PLANE('',#11949);
#755=PLANE('',#11950);
#756=PLANE('',#11951);
#757=PLANE('',#11952);
#758=PLANE('',#11953);
#759=PLANE('',#11954);
#760=PLANE('',#11955);
#761=PLANE('',#11956);
#762=PLANE('',#11957);
#763=PLANE('',#11958);
#764=PLANE('',#11959);
#765=PLANE('',#11960);
#766=PLANE('',#11961);
#767=PLANE('',#11962);
#768=PLANE('',#11963);
#769=PLANE('',#11965);
#770=PLANE('',#11967);
#771=PLANE('',#11969);
#772=PLANE('',#11971);
#773=PLANE('',#11973);
#774=PLANE('',#11975);
#775=PLANE('',#11977);
#776=PLANE('',#11981);
#777=PLANE('',#11987);
#778=PLANE('',#11988);
#779=PLANE('',#11989);
#780=PLANE('',#11990);
#781=PLANE('',#11991);
#782=PLANE('',#11992);
#783=PLANE('',#11993);
#784=PLANE('',#11994);
#785=PLANE('',#11995);
#786=PLANE('',#11996);
#787=PLANE('',#11997);
#788=PLANE('',#11998);
#789=PLANE('',#11999);
#790=PLANE('',#12000);
#791=PLANE('',#12001);
#792=PLANE('',#12002);
#793=PLANE('',#12003);
#794=PLANE('',#12004);
#795=PLANE('',#12005);
#796=PLANE('',#12006);
#797=PLANE('',#12008);
#798=PLANE('',#12010);
#799=PLANE('',#12012);
#800=PLANE('',#12014);
#801=PLANE('',#12016);
#802=PLANE('',#12018);
#803=PLANE('',#12023);
#804=PLANE('',#12025);
#805=PLANE('',#12027);
#806=PLANE('',#12028);
#807=PLANE('',#12029);
#808=PLANE('',#12030);
#809=PLANE('',#12031);
#810=PLANE('',#12032);
#811=PLANE('',#12033);
#812=PLANE('',#12034);
#813=PLANE('',#12035);
#814=PLANE('',#12036);
#815=PLANE('',#12037);
#816=PLANE('',#12038);
#817=PLANE('',#12039);
#818=PLANE('',#12040);
#819=PLANE('',#12041);
#820=PLANE('',#12042);
#821=PLANE('',#12043);
#822=PLANE('',#12044);
#823=PLANE('',#12045);
#824=PLANE('',#12046);
#825=PLANE('',#12048);
#826=PLANE('',#12050);
#827=PLANE('',#12052);
#828=PLANE('',#12054);
#829=PLANE('',#12056);
#830=PLANE('',#12058);
#831=PLANE('',#12060);
#832=PLANE('',#12062);
#833=PLANE('',#12063);
#834=PLANE('',#12064);
#835=PLANE('',#12065);
#836=PLANE('',#12066);
#837=PLANE('',#12067);
#838=PLANE('',#12068);
#839=PLANE('',#12069);
#840=PLANE('',#12070);
#841=PLANE('',#12071);
#842=PLANE('',#12072);
#843=PLANE('',#12073);
#844=PLANE('',#12074);
#845=PLANE('',#12075);
#846=PLANE('',#12076);
#847=PLANE('',#12077);
#848=PLANE('',#12078);
#849=PLANE('',#12079);
#850=PLANE('',#12080);
#851=PLANE('',#12081);
#852=PLANE('',#12083);
#853=PLANE('',#12085);
#854=PLANE('',#12087);
#855=PLANE('',#12089);
#856=PLANE('',#12091);
#857=PLANE('',#12093);
#858=PLANE('',#12095);
#859=PLANE('',#12099);
#860=PLANE('',#12101);
#861=PLANE('',#12120);
#862=PLANE('',#12121);
#863=PLANE('',#12122);
#864=PLANE('',#12123);
#865=PLANE('',#12124);
#866=PLANE('',#12125);
#867=PLANE('',#12126);
#868=PLANE('',#12127);
#869=PLANE('',#12128);
#870=PLANE('',#12129);
#871=PLANE('',#12130);
#872=PLANE('',#12131);
#873=PLANE('',#12132);
#874=PLANE('',#12133);
#875=PLANE('',#12134);
#876=PLANE('',#12135);
#877=PLANE('',#12136);
#878=PLANE('',#12137);
#879=PLANE('',#12138);
#880=PLANE('',#12139);
#881=PLANE('',#12140);
#882=PLANE('',#12141);
#883=PLANE('',#12142);
#884=PLANE('',#12143);
#885=PLANE('',#12144);
#886=PLANE('',#12145);
#887=PLANE('',#12146);
#888=PLANE('',#12147);
#889=PLANE('',#12148);
#890=PLANE('',#12149);
#891=PLANE('',#12150);
#892=PLANE('',#12151);
#893=PLANE('',#12152);
#894=PLANE('',#12153);
#895=PLANE('',#12154);
#896=PLANE('',#12155);
#897=PLANE('',#12156);
#898=PLANE('',#12157);
#899=PLANE('',#12158);
#900=PLANE('',#12159);
#901=PLANE('',#12160);
#902=PLANE('',#12161);
#903=PLANE('',#12162);
#904=PLANE('',#12163);
#905=PLANE('',#12164);
#906=PLANE('',#12165);
#907=PLANE('',#12166);
#908=PLANE('',#12167);
#909=PLANE('',#12168);
#910=PLANE('',#12169);
#911=PLANE('',#12170);
#912=PLANE('',#12171);
#913=PLANE('',#12172);
#914=PLANE('',#12173);
#915=PLANE('',#12174);
#916=PLANE('',#12175);
#917=PLANE('',#12176);
#918=PLANE('',#12177);
#919=PLANE('',#12178);
#920=PLANE('',#12179);
#921=PLANE('',#12180);
#922=PLANE('',#12181);
#923=PLANE('',#12182);
#924=PLANE('',#12183);
#925=PLANE('',#12184);
#926=PLANE('',#12185);
#927=PLANE('',#12186);
#928=PLANE('',#12187);
#929=PLANE('',#12188);
#930=PLANE('',#12189);
#931=PLANE('',#12190);
#932=PLANE('',#12191);
#933=PLANE('',#12192);
#934=PLANE('',#12193);
#935=PLANE('',#12194);
#936=PLANE('',#12195);
#937=PLANE('',#12196);
#938=PLANE('',#12197);
#939=PLANE('',#12198);
#940=PLANE('',#12199);
#941=PLANE('',#12200);
#942=PLANE('',#12201);
#943=PLANE('',#12202);
#944=PLANE('',#12203);
#945=PLANE('',#12204);
#946=PLANE('',#12205);
#947=PLANE('',#12206);
#948=PLANE('',#12207);
#949=PLANE('',#12208);
#950=PLANE('',#12209);
#951=PLANE('',#12210);
#952=PLANE('',#12211);
#953=PLANE('',#12212);
#954=PLANE('',#12213);
#955=PLANE('',#12214);
#956=PLANE('',#12215);
#957=PLANE('',#12216);
#958=PLANE('',#12217);
#959=PLANE('',#12218);
#960=PLANE('',#12219);
#961=PLANE('',#12220);
#962=PLANE('',#12221);
#963=PLANE('',#12222);
#964=PLANE('',#12223);
#965=PLANE('',#12224);
#966=PLANE('',#12225);
#967=PLANE('',#12226);
#968=PLANE('',#12227);
#969=PLANE('',#12228);
#970=PLANE('',#12229);
#971=PLANE('',#12230);
#972=PLANE('',#12231);
#973=PLANE('',#12232);
#974=PLANE('',#12233);
#975=PLANE('',#12234);
#976=PLANE('',#12235);
#977=PLANE('',#12236);
#978=PLANE('',#12237);
#979=PLANE('',#12238);
#980=PLANE('',#12239);
#981=PLANE('',#12240);
#982=PLANE('',#12241);
#983=PLANE('',#12242);
#984=PLANE('',#12243);
#985=PLANE('',#12244);
#986=PLANE('',#12245);
#987=PLANE('',#12246);
#988=PLANE('',#12247);
#989=PLANE('',#12248);
#990=PLANE('',#12249);
#991=PLANE('',#12250);
#992=PLANE('',#12251);
#993=PLANE('',#12252);
#994=PLANE('',#12257);
#995=PLANE('',#12261);
#996=PLANE('',#12267);
#997=PLANE('',#12268);
#998=PLANE('',#12269);
#999=PLANE('',#12272);
#1000=PLANE('',#12277);
#1001=PLANE('',#12278);
#1002=PLANE('',#12280);
#1003=PLANE('',#12281);
#1004=PLANE('',#12282);
#1005=PLANE('',#12283);
#1006=PLANE('',#12284);
#1007=PLANE('',#12285);
#1008=PLANE('',#12286);
#1009=PLANE('',#12287);
#1010=PLANE('',#12295);
#1011=PLANE('',#12297);
#1012=PLANE('',#12305);
#1013=PLANE('',#12313);
#1014=PLANE('',#12314);
#1015=PLANE('',#12315);
#1016=PLANE('',#12316);
#1017=PLANE('',#12317);
#1018=PLANE('',#12318);
#1019=PLANE('',#12319);
#1020=PLANE('',#12320);
#1021=PLANE('',#12321);
#1022=FACE_OUTER_BOUND('',#1642,.T.);
#1023=FACE_OUTER_BOUND('',#1643,.T.);
#1024=FACE_OUTER_BOUND('',#1644,.T.);
#1025=FACE_OUTER_BOUND('',#1645,.T.);
#1026=FACE_OUTER_BOUND('',#1646,.T.);
#1027=FACE_OUTER_BOUND('',#1647,.T.);
#1028=FACE_OUTER_BOUND('',#1648,.T.);
#1029=FACE_OUTER_BOUND('',#1649,.T.);
#1030=FACE_OUTER_BOUND('',#1650,.T.);
#1031=FACE_OUTER_BOUND('',#1651,.T.);
#1032=FACE_OUTER_BOUND('',#1652,.T.);
#1033=FACE_OUTER_BOUND('',#1659,.T.);
#1034=FACE_OUTER_BOUND('',#1666,.T.);
#1035=FACE_OUTER_BOUND('',#1667,.T.);
#1036=FACE_OUTER_BOUND('',#1668,.T.);
#1037=FACE_OUTER_BOUND('',#1669,.T.);
#1038=FACE_OUTER_BOUND('',#1670,.T.);
#1039=FACE_OUTER_BOUND('',#1671,.T.);
#1040=FACE_OUTER_BOUND('',#1672,.T.);
#1041=FACE_OUTER_BOUND('',#1673,.T.);
#1042=FACE_OUTER_BOUND('',#1674,.T.);
#1043=FACE_OUTER_BOUND('',#1675,.T.);
#1044=FACE_OUTER_BOUND('',#1676,.T.);
#1045=FACE_OUTER_BOUND('',#1677,.T.);
#1046=FACE_OUTER_BOUND('',#1678,.T.);
#1047=FACE_OUTER_BOUND('',#1679,.T.);
#1048=FACE_OUTER_BOUND('',#1680,.T.);
#1049=FACE_OUTER_BOUND('',#1682,.T.);
#1050=FACE_OUTER_BOUND('',#1684,.T.);
#1051=FACE_OUTER_BOUND('',#1685,.T.);
#1052=FACE_OUTER_BOUND('',#1686,.T.);
#1053=FACE_OUTER_BOUND('',#1688,.T.);
#1054=FACE_OUTER_BOUND('',#1690,.T.);
#1055=FACE_OUTER_BOUND('',#1691,.T.);
#1056=FACE_OUTER_BOUND('',#1692,.T.);
#1057=FACE_OUTER_BOUND('',#1694,.T.);
#1058=FACE_OUTER_BOUND('',#1696,.T.);
#1059=FACE_OUTER_BOUND('',#1697,.T.);
#1060=FACE_OUTER_BOUND('',#1698,.T.);
#1061=FACE_OUTER_BOUND('',#1700,.T.);
#1062=FACE_OUTER_BOUND('',#1702,.T.);
#1063=FACE_OUTER_BOUND('',#1703,.T.);
#1064=FACE_OUTER_BOUND('',#1704,.T.);
#1065=FACE_OUTER_BOUND('',#1705,.T.);
#1066=FACE_OUTER_BOUND('',#1706,.T.);
#1067=FACE_OUTER_BOUND('',#1707,.T.);
#1068=FACE_OUTER_BOUND('',#1708,.T.);
#1069=FACE_OUTER_BOUND('',#1709,.T.);
#1070=FACE_OUTER_BOUND('',#1712,.T.);
#1071=FACE_OUTER_BOUND('',#1713,.T.);
#1072=FACE_OUTER_BOUND('',#1719,.T.);
#1073=FACE_OUTER_BOUND('',#1720,.T.);
#1074=FACE_OUTER_BOUND('',#1721,.T.);
#1075=FACE_OUTER_BOUND('',#1727,.T.);
#1076=FACE_OUTER_BOUND('',#1728,.T.);
#1077=FACE_OUTER_BOUND('',#1731,.T.);
#1078=FACE_OUTER_BOUND('',#1732,.T.);
#1079=FACE_OUTER_BOUND('',#1733,.T.);
#1080=FACE_OUTER_BOUND('',#1734,.T.);
#1081=FACE_OUTER_BOUND('',#1735,.T.);
#1082=FACE_OUTER_BOUND('',#1736,.T.);
#1083=FACE_OUTER_BOUND('',#1737,.T.);
#1084=FACE_OUTER_BOUND('',#1738,.T.);
#1085=FACE_OUTER_BOUND('',#1739,.T.);
#1086=FACE_OUTER_BOUND('',#1740,.T.);
#1087=FACE_OUTER_BOUND('',#1742,.T.);
#1088=FACE_OUTER_BOUND('',#1743,.T.);
#1089=FACE_OUTER_BOUND('',#1749,.T.);
#1090=FACE_OUTER_BOUND('',#1750,.T.);
#1091=FACE_OUTER_BOUND('',#1752,.T.);
#1092=FACE_OUTER_BOUND('',#1753,.T.);
#1093=FACE_OUTER_BOUND('',#1754,.T.);
#1094=FACE_OUTER_BOUND('',#1755,.T.);
#1095=FACE_OUTER_BOUND('',#1756,.T.);
#1096=FACE_OUTER_BOUND('',#1757,.T.);
#1097=FACE_OUTER_BOUND('',#1758,.T.);
#1098=FACE_OUTER_BOUND('',#1759,.T.);
#1099=FACE_OUTER_BOUND('',#1760,.T.);
#1100=FACE_OUTER_BOUND('',#1761,.T.);
#1101=FACE_OUTER_BOUND('',#1762,.T.);
#1102=FACE_OUTER_BOUND('',#1764,.T.);
#1103=FACE_OUTER_BOUND('',#1765,.T.);
#1104=FACE_OUTER_BOUND('',#1767,.T.);
#1105=FACE_OUTER_BOUND('',#1768,.T.);
#1106=FACE_OUTER_BOUND('',#1769,.T.);
#1107=FACE_OUTER_BOUND('',#1770,.T.);
#1108=FACE_OUTER_BOUND('',#1771,.T.);
#1109=FACE_OUTER_BOUND('',#1772,.T.);
#1110=FACE_OUTER_BOUND('',#1773,.T.);
#1111=FACE_OUTER_BOUND('',#1774,.T.);
#1112=FACE_OUTER_BOUND('',#1775,.T.);
#1113=FACE_OUTER_BOUND('',#1776,.T.);
#1114=FACE_OUTER_BOUND('',#1778,.T.);
#1115=FACE_OUTER_BOUND('',#1779,.T.);
#1116=FACE_OUTER_BOUND('',#1781,.T.);
#1117=FACE_OUTER_BOUND('',#1782,.T.);
#1118=FACE_OUTER_BOUND('',#1783,.T.);
#1119=FACE_OUTER_BOUND('',#1784,.T.);
#1120=FACE_OUTER_BOUND('',#1785,.T.);
#1121=FACE_OUTER_BOUND('',#1786,.T.);
#1122=FACE_OUTER_BOUND('',#1787,.T.);
#1123=FACE_OUTER_BOUND('',#1788,.T.);
#1124=FACE_OUTER_BOUND('',#1789,.T.);
#1125=FACE_OUTER_BOUND('',#1790,.T.);
#1126=FACE_OUTER_BOUND('',#1792,.T.);
#1127=FACE_OUTER_BOUND('',#1793,.T.);
#1128=FACE_OUTER_BOUND('',#1795,.T.);
#1129=FACE_OUTER_BOUND('',#1796,.T.);
#1130=FACE_OUTER_BOUND('',#1797,.T.);
#1131=FACE_OUTER_BOUND('',#1798,.T.);
#1132=FACE_OUTER_BOUND('',#1799,.T.);
#1133=FACE_OUTER_BOUND('',#1800,.T.);
#1134=FACE_OUTER_BOUND('',#1801,.T.);
#1135=FACE_OUTER_BOUND('',#1802,.T.);
#1136=FACE_OUTER_BOUND('',#1803,.T.);
#1137=FACE_OUTER_BOUND('',#1804,.T.);
#1138=FACE_OUTER_BOUND('',#1806,.T.);
#1139=FACE_OUTER_BOUND('',#1807,.T.);
#1140=FACE_OUTER_BOUND('',#1809,.T.);
#1141=FACE_OUTER_BOUND('',#1810,.T.);
#1142=FACE_OUTER_BOUND('',#1811,.T.);
#1143=FACE_OUTER_BOUND('',#1812,.T.);
#1144=FACE_OUTER_BOUND('',#1813,.T.);
#1145=FACE_OUTER_BOUND('',#1814,.T.);
#1146=FACE_OUTER_BOUND('',#1815,.T.);
#1147=FACE_OUTER_BOUND('',#1816,.T.);
#1148=FACE_OUTER_BOUND('',#1819,.T.);
#1149=FACE_OUTER_BOUND('',#1820,.T.);
#1150=FACE_OUTER_BOUND('',#1821,.T.);
#1151=FACE_OUTER_BOUND('',#1822,.T.);
#1152=FACE_OUTER_BOUND('',#1823,.T.);
#1153=FACE_OUTER_BOUND('',#1824,.T.);
#1154=FACE_OUTER_BOUND('',#1825,.T.);
#1155=FACE_OUTER_BOUND('',#1829,.T.);
#1156=FACE_OUTER_BOUND('',#1830,.T.);
#1157=FACE_OUTER_BOUND('',#1831,.T.);
#1158=FACE_OUTER_BOUND('',#1832,.T.);
#1159=FACE_OUTER_BOUND('',#1833,.T.);
#1160=FACE_OUTER_BOUND('',#1834,.T.);
#1161=FACE_OUTER_BOUND('',#1835,.T.);
#1162=FACE_OUTER_BOUND('',#1836,.T.);
#1163=FACE_OUTER_BOUND('',#1837,.T.);
#1164=FACE_OUTER_BOUND('',#1838,.T.);
#1165=FACE_OUTER_BOUND('',#1839,.T.);
#1166=FACE_OUTER_BOUND('',#1840,.T.);
#1167=FACE_OUTER_BOUND('',#1841,.T.);
#1168=FACE_OUTER_BOUND('',#1842,.T.);
#1169=FACE_OUTER_BOUND('',#1843,.T.);
#1170=FACE_OUTER_BOUND('',#1844,.T.);
#1171=FACE_OUTER_BOUND('',#1848,.T.);
#1172=FACE_OUTER_BOUND('',#1849,.T.);
#1173=FACE_OUTER_BOUND('',#1851,.T.);
#1174=FACE_OUTER_BOUND('',#1854,.T.);
#1175=FACE_OUTER_BOUND('',#1856,.T.);
#1176=FACE_OUTER_BOUND('',#1857,.T.);
#1177=FACE_OUTER_BOUND('',#1858,.T.);
#1178=FACE_OUTER_BOUND('',#1865,.T.);
#1179=FACE_OUTER_BOUND('',#1866,.T.);
#1180=FACE_OUTER_BOUND('',#1867,.T.);
#1181=FACE_OUTER_BOUND('',#1868,.T.);
#1182=FACE_OUTER_BOUND('',#1869,.T.);
#1183=FACE_OUTER_BOUND('',#1871,.T.);
#1184=FACE_OUTER_BOUND('',#1873,.T.);
#1185=FACE_OUTER_BOUND('',#1874,.T.);
#1186=FACE_OUTER_BOUND('',#1876,.T.);
#1187=FACE_OUTER_BOUND('',#1883,.T.);
#1188=FACE_OUTER_BOUND('',#1884,.T.);
#1189=FACE_OUTER_BOUND('',#1885,.T.);
#1190=FACE_OUTER_BOUND('',#1887,.T.);
#1191=FACE_OUTER_BOUND('',#1889,.T.);
#1192=FACE_OUTER_BOUND('',#1890,.T.);
#1193=FACE_OUTER_BOUND('',#1891,.T.);
#1194=FACE_OUTER_BOUND('',#1892,.T.);
#1195=FACE_OUTER_BOUND('',#1893,.T.);
#1196=FACE_OUTER_BOUND('',#1894,.T.);
#1197=FACE_OUTER_BOUND('',#1895,.T.);
#1198=FACE_OUTER_BOUND('',#1896,.T.);
#1199=FACE_OUTER_BOUND('',#1897,.T.);
#1200=FACE_OUTER_BOUND('',#1898,.T.);
#1201=FACE_OUTER_BOUND('',#1899,.T.);
#1202=FACE_OUTER_BOUND('',#1900,.T.);
#1203=FACE_OUTER_BOUND('',#1901,.T.);
#1204=FACE_OUTER_BOUND('',#1902,.T.);
#1205=FACE_OUTER_BOUND('',#1904,.T.);
#1206=FACE_OUTER_BOUND('',#1905,.T.);
#1207=FACE_OUTER_BOUND('',#1906,.T.);
#1208=FACE_OUTER_BOUND('',#1907,.T.);
#1209=FACE_OUTER_BOUND('',#1908,.T.);
#1210=FACE_OUTER_BOUND('',#1909,.T.);
#1211=FACE_OUTER_BOUND('',#1910,.T.);
#1212=FACE_OUTER_BOUND('',#1911,.T.);
#1213=FACE_OUTER_BOUND('',#1912,.T.);
#1214=FACE_OUTER_BOUND('',#1913,.T.);
#1215=FACE_OUTER_BOUND('',#1914,.T.);
#1216=FACE_OUTER_BOUND('',#1915,.T.);
#1217=FACE_OUTER_BOUND('',#1916,.T.);
#1218=FACE_OUTER_BOUND('',#1917,.T.);
#1219=FACE_OUTER_BOUND('',#1918,.T.);
#1220=FACE_OUTER_BOUND('',#1919,.T.);
#1221=FACE_OUTER_BOUND('',#1921,.T.);
#1222=FACE_OUTER_BOUND('',#1922,.T.);
#1223=FACE_OUTER_BOUND('',#1923,.T.);
#1224=FACE_OUTER_BOUND('',#1924,.T.);
#1225=FACE_OUTER_BOUND('',#1925,.T.);
#1226=FACE_OUTER_BOUND('',#1926,.T.);
#1227=FACE_OUTER_BOUND('',#1927,.T.);
#1228=FACE_OUTER_BOUND('',#1928,.T.);
#1229=FACE_OUTER_BOUND('',#1929,.T.);
#1230=FACE_OUTER_BOUND('',#1930,.T.);
#1231=FACE_OUTER_BOUND('',#1932,.T.);
#1232=FACE_OUTER_BOUND('',#1934,.T.);
#1233=FACE_OUTER_BOUND('',#1935,.T.);
#1234=FACE_OUTER_BOUND('',#1936,.T.);
#1235=FACE_OUTER_BOUND('',#1937,.T.);
#1236=FACE_OUTER_BOUND('',#1938,.T.);
#1237=FACE_OUTER_BOUND('',#1939,.T.);
#1238=FACE_OUTER_BOUND('',#1940,.T.);
#1239=FACE_OUTER_BOUND('',#1941,.T.);
#1240=FACE_OUTER_BOUND('',#1943,.T.);
#1241=FACE_OUTER_BOUND('',#1945,.T.);
#1242=FACE_OUTER_BOUND('',#1947,.T.);
#1243=FACE_OUTER_BOUND('',#1949,.T.);
#1244=FACE_OUTER_BOUND('',#1950,.T.);
#1245=FACE_OUTER_BOUND('',#1951,.T.);
#1246=FACE_OUTER_BOUND('',#1952,.T.);
#1247=FACE_OUTER_BOUND('',#1953,.T.);
#1248=FACE_OUTER_BOUND('',#1954,.T.);
#1249=FACE_OUTER_BOUND('',#1955,.T.);
#1250=FACE_OUTER_BOUND('',#1957,.T.);
#1251=FACE_OUTER_BOUND('',#1959,.T.);
#1252=FACE_OUTER_BOUND('',#1961,.T.);
#1253=FACE_OUTER_BOUND('',#1963,.T.);
#1254=FACE_OUTER_BOUND('',#1964,.T.);
#1255=FACE_OUTER_BOUND('',#1966,.T.);
#1256=FACE_OUTER_BOUND('',#1967,.T.);
#1257=FACE_OUTER_BOUND('',#1969,.T.);
#1258=FACE_OUTER_BOUND('',#1970,.T.);
#1259=FACE_OUTER_BOUND('',#1971,.T.);
#1260=FACE_OUTER_BOUND('',#1972,.T.);
#1261=FACE_OUTER_BOUND('',#1974,.T.);
#1262=FACE_OUTER_BOUND('',#1976,.T.);
#1263=FACE_OUTER_BOUND('',#1978,.T.);
#1264=FACE_OUTER_BOUND('',#1980,.T.);
#1265=FACE_OUTER_BOUND('',#1981,.T.);
#1266=FACE_OUTER_BOUND('',#1982,.T.);
#1267=FACE_OUTER_BOUND('',#1983,.T.);
#1268=FACE_OUTER_BOUND('',#1985,.T.);
#1269=FACE_OUTER_BOUND('',#1987,.T.);
#1270=FACE_OUTER_BOUND('',#1989,.T.);
#1271=FACE_OUTER_BOUND('',#1991,.T.);
#1272=FACE_OUTER_BOUND('',#1992,.T.);
#1273=FACE_OUTER_BOUND('',#1993,.T.);
#1274=FACE_OUTER_BOUND('',#1995,.T.);
#1275=FACE_OUTER_BOUND('',#1997,.T.);
#1276=FACE_OUTER_BOUND('',#1998,.T.);
#1277=FACE_OUTER_BOUND('',#1999,.T.);
#1278=FACE_OUTER_BOUND('',#2000,.T.);
#1279=FACE_OUTER_BOUND('',#2001,.T.);
#1280=FACE_OUTER_BOUND('',#2002,.T.);
#1281=FACE_OUTER_BOUND('',#2003,.T.);
#1282=FACE_OUTER_BOUND('',#2004,.T.);
#1283=FACE_OUTER_BOUND('',#2006,.T.);
#1284=FACE_OUTER_BOUND('',#2007,.T.);
#1285=FACE_OUTER_BOUND('',#2008,.T.);
#1286=FACE_OUTER_BOUND('',#2009,.T.);
#1287=FACE_OUTER_BOUND('',#2010,.T.);
#1288=FACE_OUTER_BOUND('',#2011,.T.);
#1289=FACE_OUTER_BOUND('',#2013,.T.);
#1290=FACE_OUTER_BOUND('',#2014,.T.);
#1291=FACE_OUTER_BOUND('',#2015,.T.);
#1292=FACE_OUTER_BOUND('',#2016,.T.);
#1293=FACE_OUTER_BOUND('',#2017,.T.);
#1294=FACE_OUTER_BOUND('',#2018,.T.);
#1295=FACE_OUTER_BOUND('',#2019,.T.);
#1296=FACE_OUTER_BOUND('',#2020,.T.);
#1297=FACE_OUTER_BOUND('',#2021,.T.);
#1298=FACE_OUTER_BOUND('',#2022,.T.);
#1299=FACE_OUTER_BOUND('',#2023,.T.);
#1300=FACE_OUTER_BOUND('',#2024,.T.);
#1301=FACE_OUTER_BOUND('',#2025,.T.);
#1302=FACE_OUTER_BOUND('',#2026,.T.);
#1303=FACE_OUTER_BOUND('',#2027,.T.);
#1304=FACE_OUTER_BOUND('',#2028,.T.);
#1305=FACE_OUTER_BOUND('',#2029,.T.);
#1306=FACE_OUTER_BOUND('',#2030,.T.);
#1307=FACE_OUTER_BOUND('',#2031,.T.);
#1308=FACE_OUTER_BOUND('',#2032,.T.);
#1309=FACE_OUTER_BOUND('',#2033,.T.);
#1310=FACE_OUTER_BOUND('',#2034,.T.);
#1311=FACE_OUTER_BOUND('',#2035,.T.);
#1312=FACE_OUTER_BOUND('',#2036,.T.);
#1313=FACE_OUTER_BOUND('',#2037,.T.);
#1314=FACE_OUTER_BOUND('',#2038,.T.);
#1315=FACE_OUTER_BOUND('',#2039,.T.);
#1316=FACE_OUTER_BOUND('',#2040,.T.);
#1317=FACE_OUTER_BOUND('',#2042,.T.);
#1318=FACE_OUTER_BOUND('',#2043,.T.);
#1319=FACE_OUTER_BOUND('',#2044,.T.);
#1320=FACE_OUTER_BOUND('',#2045,.T.);
#1321=FACE_OUTER_BOUND('',#2046,.T.);
#1322=FACE_OUTER_BOUND('',#2047,.T.);
#1323=FACE_OUTER_BOUND('',#2048,.T.);
#1324=FACE_OUTER_BOUND('',#2049,.T.);
#1325=FACE_OUTER_BOUND('',#2050,.T.);
#1326=FACE_OUTER_BOUND('',#2051,.T.);
#1327=FACE_OUTER_BOUND('',#2052,.T.);
#1328=FACE_OUTER_BOUND('',#2053,.T.);
#1329=FACE_OUTER_BOUND('',#2054,.T.);
#1330=FACE_OUTER_BOUND('',#2055,.T.);
#1331=FACE_OUTER_BOUND('',#2056,.T.);
#1332=FACE_OUTER_BOUND('',#2057,.T.);
#1333=FACE_OUTER_BOUND('',#2058,.T.);
#1334=FACE_OUTER_BOUND('',#2059,.T.);
#1335=FACE_OUTER_BOUND('',#2060,.T.);
#1336=FACE_OUTER_BOUND('',#2061,.T.);
#1337=FACE_OUTER_BOUND('',#2062,.T.);
#1338=FACE_OUTER_BOUND('',#2063,.T.);
#1339=FACE_OUTER_BOUND('',#2064,.T.);
#1340=FACE_OUTER_BOUND('',#2065,.T.);
#1341=FACE_OUTER_BOUND('',#2066,.T.);
#1342=FACE_OUTER_BOUND('',#2067,.T.);
#1343=FACE_OUTER_BOUND('',#2068,.T.);
#1344=FACE_OUTER_BOUND('',#2069,.T.);
#1345=FACE_OUTER_BOUND('',#2070,.T.);
#1346=FACE_OUTER_BOUND('',#2071,.T.);
#1347=FACE_OUTER_BOUND('',#2072,.T.);
#1348=FACE_OUTER_BOUND('',#2073,.T.);
#1349=FACE_OUTER_BOUND('',#2074,.T.);
#1350=FACE_OUTER_BOUND('',#2075,.T.);
#1351=FACE_OUTER_BOUND('',#2076,.T.);
#1352=FACE_OUTER_BOUND('',#2077,.T.);
#1353=FACE_OUTER_BOUND('',#2078,.T.);
#1354=FACE_OUTER_BOUND('',#2079,.T.);
#1355=FACE_OUTER_BOUND('',#2080,.T.);
#1356=FACE_OUTER_BOUND('',#2081,.T.);
#1357=FACE_OUTER_BOUND('',#2082,.T.);
#1358=FACE_OUTER_BOUND('',#2083,.T.);
#1359=FACE_OUTER_BOUND('',#2084,.T.);
#1360=FACE_OUTER_BOUND('',#2085,.T.);
#1361=FACE_OUTER_BOUND('',#2086,.T.);
#1362=FACE_OUTER_BOUND('',#2087,.T.);
#1363=FACE_OUTER_BOUND('',#2088,.T.);
#1364=FACE_OUTER_BOUND('',#2089,.T.);
#1365=FACE_OUTER_BOUND('',#2090,.T.);
#1366=FACE_OUTER_BOUND('',#2091,.T.);
#1367=FACE_OUTER_BOUND('',#2092,.T.);
#1368=FACE_OUTER_BOUND('',#2093,.T.);
#1369=FACE_OUTER_BOUND('',#2094,.T.);
#1370=FACE_OUTER_BOUND('',#2095,.T.);
#1371=FACE_OUTER_BOUND('',#2096,.T.);
#1372=FACE_OUTER_BOUND('',#2098,.T.);
#1373=FACE_OUTER_BOUND('',#2100,.T.);
#1374=FACE_OUTER_BOUND('',#2101,.T.);
#1375=FACE_OUTER_BOUND('',#2103,.T.);
#1376=FACE_OUTER_BOUND('',#2104,.T.);
#1377=FACE_OUTER_BOUND('',#2105,.T.);
#1378=FACE_OUTER_BOUND('',#2106,.T.);
#1379=FACE_OUTER_BOUND('',#2107,.T.);
#1380=FACE_OUTER_BOUND('',#2108,.T.);
#1381=FACE_OUTER_BOUND('',#2109,.T.);
#1382=FACE_OUTER_BOUND('',#2110,.T.);
#1383=FACE_OUTER_BOUND('',#2111,.T.);
#1384=FACE_OUTER_BOUND('',#2112,.T.);
#1385=FACE_OUTER_BOUND('',#2113,.T.);
#1386=FACE_OUTER_BOUND('',#2114,.T.);
#1387=FACE_OUTER_BOUND('',#2115,.T.);
#1388=FACE_OUTER_BOUND('',#2116,.T.);
#1389=FACE_OUTER_BOUND('',#2117,.T.);
#1390=FACE_OUTER_BOUND('',#2118,.T.);
#1391=FACE_OUTER_BOUND('',#2119,.T.);
#1392=FACE_OUTER_BOUND('',#2120,.T.);
#1393=FACE_OUTER_BOUND('',#2121,.T.);
#1394=FACE_OUTER_BOUND('',#2122,.T.);
#1395=FACE_OUTER_BOUND('',#2123,.T.);
#1396=FACE_OUTER_BOUND('',#2124,.T.);
#1397=FACE_OUTER_BOUND('',#2125,.T.);
#1398=FACE_OUTER_BOUND('',#2126,.T.);
#1399=FACE_OUTER_BOUND('',#2127,.T.);
#1400=FACE_OUTER_BOUND('',#2128,.T.);
#1401=FACE_OUTER_BOUND('',#2130,.T.);
#1402=FACE_OUTER_BOUND('',#2131,.T.);
#1403=FACE_OUTER_BOUND('',#2132,.T.);
#1404=FACE_OUTER_BOUND('',#2133,.T.);
#1405=FACE_OUTER_BOUND('',#2134,.T.);
#1406=FACE_OUTER_BOUND('',#2135,.T.);
#1407=FACE_OUTER_BOUND('',#2136,.T.);
#1408=FACE_OUTER_BOUND('',#2137,.T.);
#1409=FACE_OUTER_BOUND('',#2138,.T.);
#1410=FACE_OUTER_BOUND('',#2139,.T.);
#1411=FACE_OUTER_BOUND('',#2140,.T.);
#1412=FACE_OUTER_BOUND('',#2141,.T.);
#1413=FACE_OUTER_BOUND('',#2142,.T.);
#1414=FACE_OUTER_BOUND('',#2143,.T.);
#1415=FACE_OUTER_BOUND('',#2144,.T.);
#1416=FACE_OUTER_BOUND('',#2145,.T.);
#1417=FACE_OUTER_BOUND('',#2146,.T.);
#1418=FACE_OUTER_BOUND('',#2147,.T.);
#1419=FACE_OUTER_BOUND('',#2148,.T.);
#1420=FACE_OUTER_BOUND('',#2149,.T.);
#1421=FACE_OUTER_BOUND('',#2150,.T.);
#1422=FACE_OUTER_BOUND('',#2151,.T.);
#1423=FACE_OUTER_BOUND('',#2152,.T.);
#1424=FACE_OUTER_BOUND('',#2153,.T.);
#1425=FACE_OUTER_BOUND('',#2154,.T.);
#1426=FACE_OUTER_BOUND('',#2155,.T.);
#1427=FACE_OUTER_BOUND('',#2156,.T.);
#1428=FACE_OUTER_BOUND('',#2157,.T.);
#1429=FACE_OUTER_BOUND('',#2158,.T.);
#1430=FACE_OUTER_BOUND('',#2159,.T.);
#1431=FACE_OUTER_BOUND('',#2160,.T.);
#1432=FACE_OUTER_BOUND('',#2161,.T.);
#1433=FACE_OUTER_BOUND('',#2162,.T.);
#1434=FACE_OUTER_BOUND('',#2163,.T.);
#1435=FACE_OUTER_BOUND('',#2164,.T.);
#1436=FACE_OUTER_BOUND('',#2165,.T.);
#1437=FACE_OUTER_BOUND('',#2166,.T.);
#1438=FACE_OUTER_BOUND('',#2167,.T.);
#1439=FACE_OUTER_BOUND('',#2168,.T.);
#1440=FACE_OUTER_BOUND('',#2169,.T.);
#1441=FACE_OUTER_BOUND('',#2170,.T.);
#1442=FACE_OUTER_BOUND('',#2171,.T.);
#1443=FACE_OUTER_BOUND('',#2172,.T.);
#1444=FACE_OUTER_BOUND('',#2173,.T.);
#1445=FACE_OUTER_BOUND('',#2174,.T.);
#1446=FACE_OUTER_BOUND('',#2175,.T.);
#1447=FACE_OUTER_BOUND('',#2176,.T.);
#1448=FACE_OUTER_BOUND('',#2177,.T.);
#1449=FACE_OUTER_BOUND('',#2178,.T.);
#1450=FACE_OUTER_BOUND('',#2179,.T.);
#1451=FACE_OUTER_BOUND('',#2180,.T.);
#1452=FACE_OUTER_BOUND('',#2181,.T.);
#1453=FACE_OUTER_BOUND('',#2182,.T.);
#1454=FACE_OUTER_BOUND('',#2183,.T.);
#1455=FACE_OUTER_BOUND('',#2184,.T.);
#1456=FACE_OUTER_BOUND('',#2185,.T.);
#1457=FACE_OUTER_BOUND('',#2186,.T.);
#1458=FACE_OUTER_BOUND('',#2188,.T.);
#1459=FACE_OUTER_BOUND('',#2190,.T.);
#1460=FACE_OUTER_BOUND('',#2191,.T.);
#1461=FACE_OUTER_BOUND('',#2192,.T.);
#1462=FACE_OUTER_BOUND('',#2193,.T.);
#1463=FACE_OUTER_BOUND('',#2194,.T.);
#1464=FACE_OUTER_BOUND('',#2195,.T.);
#1465=FACE_OUTER_BOUND('',#2196,.T.);
#1466=FACE_OUTER_BOUND('',#2197,.T.);
#1467=FACE_OUTER_BOUND('',#2198,.T.);
#1468=FACE_OUTER_BOUND('',#2199,.T.);
#1469=FACE_OUTER_BOUND('',#2200,.T.);
#1470=FACE_OUTER_BOUND('',#2201,.T.);
#1471=FACE_OUTER_BOUND('',#2202,.T.);
#1472=FACE_OUTER_BOUND('',#2203,.T.);
#1473=FACE_OUTER_BOUND('',#2204,.T.);
#1474=FACE_OUTER_BOUND('',#2205,.T.);
#1475=FACE_OUTER_BOUND('',#2206,.T.);
#1476=FACE_OUTER_BOUND('',#2207,.T.);
#1477=FACE_OUTER_BOUND('',#2208,.T.);
#1478=FACE_OUTER_BOUND('',#2209,.T.);
#1479=FACE_OUTER_BOUND('',#2210,.T.);
#1480=FACE_OUTER_BOUND('',#2211,.T.);
#1481=FACE_OUTER_BOUND('',#2212,.T.);
#1482=FACE_OUTER_BOUND('',#2213,.T.);
#1483=FACE_OUTER_BOUND('',#2214,.T.);
#1484=FACE_OUTER_BOUND('',#2215,.T.);
#1485=FACE_OUTER_BOUND('',#2216,.T.);
#1486=FACE_OUTER_BOUND('',#2217,.T.);
#1487=FACE_OUTER_BOUND('',#2218,.T.);
#1488=FACE_OUTER_BOUND('',#2219,.T.);
#1489=FACE_OUTER_BOUND('',#2220,.T.);
#1490=FACE_OUTER_BOUND('',#2221,.T.);
#1491=FACE_OUTER_BOUND('',#2222,.T.);
#1492=FACE_OUTER_BOUND('',#2223,.T.);
#1493=FACE_OUTER_BOUND('',#2224,.T.);
#1494=FACE_OUTER_BOUND('',#2225,.T.);
#1495=FACE_OUTER_BOUND('',#2226,.T.);
#1496=FACE_OUTER_BOUND('',#2227,.T.);
#1497=FACE_OUTER_BOUND('',#2228,.T.);
#1498=FACE_OUTER_BOUND('',#2229,.T.);
#1499=FACE_OUTER_BOUND('',#2230,.T.);
#1500=FACE_OUTER_BOUND('',#2231,.T.);
#1501=FACE_OUTER_BOUND('',#2232,.T.);
#1502=FACE_OUTER_BOUND('',#2233,.T.);
#1503=FACE_OUTER_BOUND('',#2234,.T.);
#1504=FACE_OUTER_BOUND('',#2235,.T.);
#1505=FACE_OUTER_BOUND('',#2236,.T.);
#1506=FACE_OUTER_BOUND('',#2237,.T.);
#1507=FACE_OUTER_BOUND('',#2238,.T.);
#1508=FACE_OUTER_BOUND('',#2239,.T.);
#1509=FACE_OUTER_BOUND('',#2240,.T.);
#1510=FACE_OUTER_BOUND('',#2241,.T.);
#1511=FACE_OUTER_BOUND('',#2242,.T.);
#1512=FACE_OUTER_BOUND('',#2243,.T.);
#1513=FACE_OUTER_BOUND('',#2244,.T.);
#1514=FACE_OUTER_BOUND('',#2245,.T.);
#1515=FACE_OUTER_BOUND('',#2246,.T.);
#1516=FACE_OUTER_BOUND('',#2247,.T.);
#1517=FACE_OUTER_BOUND('',#2248,.T.);
#1518=FACE_OUTER_BOUND('',#2249,.T.);
#1519=FACE_OUTER_BOUND('',#2250,.T.);
#1520=FACE_OUTER_BOUND('',#2251,.T.);
#1521=FACE_OUTER_BOUND('',#2252,.T.);
#1522=FACE_OUTER_BOUND('',#2253,.T.);
#1523=FACE_OUTER_BOUND('',#2254,.T.);
#1524=FACE_OUTER_BOUND('',#2255,.T.);
#1525=FACE_OUTER_BOUND('',#2256,.T.);
#1526=FACE_OUTER_BOUND('',#2257,.T.);
#1527=FACE_OUTER_BOUND('',#2258,.T.);
#1528=FACE_OUTER_BOUND('',#2259,.T.);
#1529=FACE_OUTER_BOUND('',#2260,.T.);
#1530=FACE_OUTER_BOUND('',#2261,.T.);
#1531=FACE_OUTER_BOUND('',#2262,.T.);
#1532=FACE_OUTER_BOUND('',#2263,.T.);
#1533=FACE_OUTER_BOUND('',#2264,.T.);
#1534=FACE_OUTER_BOUND('',#2265,.T.);
#1535=FACE_OUTER_BOUND('',#2266,.T.);
#1536=FACE_OUTER_BOUND('',#2267,.T.);
#1537=FACE_OUTER_BOUND('',#2268,.T.);
#1538=FACE_OUTER_BOUND('',#2269,.T.);
#1539=FACE_OUTER_BOUND('',#2270,.T.);
#1540=FACE_OUTER_BOUND('',#2271,.T.);
#1541=FACE_OUTER_BOUND('',#2272,.T.);
#1542=FACE_OUTER_BOUND('',#2273,.T.);
#1543=FACE_OUTER_BOUND('',#2274,.T.);
#1544=FACE_OUTER_BOUND('',#2275,.T.);
#1545=FACE_OUTER_BOUND('',#2276,.T.);
#1546=FACE_OUTER_BOUND('',#2277,.T.);
#1547=FACE_OUTER_BOUND('',#2278,.T.);
#1548=FACE_OUTER_BOUND('',#2279,.T.);
#1549=FACE_OUTER_BOUND('',#2280,.T.);
#1550=FACE_OUTER_BOUND('',#2281,.T.);
#1551=FACE_OUTER_BOUND('',#2282,.T.);
#1552=FACE_OUTER_BOUND('',#2283,.T.);
#1553=FACE_OUTER_BOUND('',#2284,.T.);
#1554=FACE_OUTER_BOUND('',#2285,.T.);
#1555=FACE_OUTER_BOUND('',#2286,.T.);
#1556=FACE_OUTER_BOUND('',#2287,.T.);
#1557=FACE_OUTER_BOUND('',#2288,.T.);
#1558=FACE_OUTER_BOUND('',#2289,.T.);
#1559=FACE_OUTER_BOUND('',#2290,.T.);
#1560=FACE_OUTER_BOUND('',#2291,.T.);
#1561=FACE_OUTER_BOUND('',#2292,.T.);
#1562=FACE_OUTER_BOUND('',#2293,.T.);
#1563=FACE_OUTER_BOUND('',#2294,.T.);
#1564=FACE_OUTER_BOUND('',#2295,.T.);
#1565=FACE_OUTER_BOUND('',#2296,.T.);
#1566=FACE_OUTER_BOUND('',#2297,.T.);
#1567=FACE_OUTER_BOUND('',#2298,.T.);
#1568=FACE_OUTER_BOUND('',#2299,.T.);
#1569=FACE_OUTER_BOUND('',#2300,.T.);
#1570=FACE_OUTER_BOUND('',#2301,.T.);
#1571=FACE_OUTER_BOUND('',#2302,.T.);
#1572=FACE_OUTER_BOUND('',#2303,.T.);
#1573=FACE_OUTER_BOUND('',#2304,.T.);
#1574=FACE_OUTER_BOUND('',#2305,.T.);
#1575=FACE_OUTER_BOUND('',#2306,.T.);
#1576=FACE_OUTER_BOUND('',#2307,.T.);
#1577=FACE_OUTER_BOUND('',#2308,.T.);
#1578=FACE_OUTER_BOUND('',#2309,.T.);
#1579=FACE_OUTER_BOUND('',#2310,.T.);
#1580=FACE_OUTER_BOUND('',#2311,.T.);
#1581=FACE_OUTER_BOUND('',#2312,.T.);
#1582=FACE_OUTER_BOUND('',#2313,.T.);
#1583=FACE_OUTER_BOUND('',#2314,.T.);
#1584=FACE_OUTER_BOUND('',#2315,.T.);
#1585=FACE_OUTER_BOUND('',#2316,.T.);
#1586=FACE_OUTER_BOUND('',#2317,.T.);
#1587=FACE_OUTER_BOUND('',#2318,.T.);
#1588=FACE_OUTER_BOUND('',#2319,.T.);
#1589=FACE_OUTER_BOUND('',#2320,.T.);
#1590=FACE_OUTER_BOUND('',#2321,.T.);
#1591=FACE_OUTER_BOUND('',#2322,.T.);
#1592=FACE_OUTER_BOUND('',#2323,.T.);
#1593=FACE_OUTER_BOUND('',#2324,.T.);
#1594=FACE_OUTER_BOUND('',#2325,.T.);
#1595=FACE_OUTER_BOUND('',#2326,.T.);
#1596=FACE_OUTER_BOUND('',#2327,.T.);
#1597=FACE_OUTER_BOUND('',#2328,.T.);
#1598=FACE_OUTER_BOUND('',#2329,.T.);
#1599=FACE_OUTER_BOUND('',#2330,.T.);
#1600=FACE_OUTER_BOUND('',#2331,.T.);
#1601=FACE_OUTER_BOUND('',#2332,.T.);
#1602=FACE_OUTER_BOUND('',#2333,.T.);
#1603=FACE_OUTER_BOUND('',#2334,.T.);
#1604=FACE_OUTER_BOUND('',#2335,.T.);
#1605=FACE_OUTER_BOUND('',#2336,.T.);
#1606=FACE_OUTER_BOUND('',#2337,.T.);
#1607=FACE_OUTER_BOUND('',#2338,.T.);
#1608=FACE_OUTER_BOUND('',#2339,.T.);
#1609=FACE_OUTER_BOUND('',#2340,.T.);
#1610=FACE_OUTER_BOUND('',#2341,.T.);
#1611=FACE_OUTER_BOUND('',#2342,.T.);
#1612=FACE_OUTER_BOUND('',#2343,.T.);
#1613=FACE_OUTER_BOUND('',#2344,.T.);
#1614=FACE_OUTER_BOUND('',#2345,.T.);
#1615=FACE_OUTER_BOUND('',#2346,.T.);
#1616=FACE_OUTER_BOUND('',#2347,.T.);
#1617=FACE_OUTER_BOUND('',#2348,.T.);
#1618=FACE_OUTER_BOUND('',#2349,.T.);
#1619=FACE_OUTER_BOUND('',#2350,.T.);
#1620=FACE_OUTER_BOUND('',#2351,.T.);
#1621=FACE_OUTER_BOUND('',#2353,.T.);
#1622=FACE_OUTER_BOUND('',#2354,.T.);
#1623=FACE_OUTER_BOUND('',#2355,.T.);
#1624=FACE_OUTER_BOUND('',#2356,.T.);
#1625=FACE_OUTER_BOUND('',#2357,.T.);
#1626=FACE_OUTER_BOUND('',#2358,.T.);
#1627=FACE_OUTER_BOUND('',#2359,.T.);
#1628=FACE_OUTER_BOUND('',#2360,.T.);
#1629=FACE_OUTER_BOUND('',#2361,.T.);
#1630=FACE_OUTER_BOUND('',#2363,.T.);
#1631=FACE_OUTER_BOUND('',#2364,.T.);
#1632=FACE_OUTER_BOUND('',#2365,.T.);
#1633=FACE_OUTER_BOUND('',#2366,.T.);
#1634=FACE_OUTER_BOUND('',#2367,.T.);
#1635=FACE_OUTER_BOUND('',#2368,.T.);
#1636=FACE_OUTER_BOUND('',#2369,.T.);
#1637=FACE_OUTER_BOUND('',#2370,.T.);
#1638=FACE_OUTER_BOUND('',#2371,.T.);
#1639=FACE_OUTER_BOUND('',#2372,.T.);
#1640=FACE_OUTER_BOUND('',#2373,.T.);
#1641=FACE_OUTER_BOUND('',#2374,.T.);
#1642=EDGE_LOOP('',(#7346,#7347,#7348,#7349));
#1643=EDGE_LOOP('',(#7350,#7351,#7352,#7353));
#1644=EDGE_LOOP('',(#7354,#7355,#7356,#7357));
#1645=EDGE_LOOP('',(#7358,#7359,#7360,#7361));
#1646=EDGE_LOOP('',(#7362,#7363,#7364,#7365));
#1647=EDGE_LOOP('',(#7366,#7367,#7368,#7369));
#1648=EDGE_LOOP('',(#7370,#7371,#7372,#7373));
#1649=EDGE_LOOP('',(#7374,#7375,#7376,#7377));
#1650=EDGE_LOOP('',(#7378,#7379,#7380,#7381));
#1651=EDGE_LOOP('',(#7382,#7383,#7384,#7385));
#1652=EDGE_LOOP('',(#7386,#7387,#7388,#7389));
#1653=EDGE_LOOP('',(#7390));
#1654=EDGE_LOOP('',(#7391));
#1655=EDGE_LOOP('',(#7392));
#1656=EDGE_LOOP('',(#7393));
#1657=EDGE_LOOP('',(#7394));
#1658=EDGE_LOOP('',(#7395));
#1659=EDGE_LOOP('',(#7396,#7397,#7398,#7399));
#1660=EDGE_LOOP('',(#7400));
#1661=EDGE_LOOP('',(#7401));
#1662=EDGE_LOOP('',(#7402));
#1663=EDGE_LOOP('',(#7403));
#1664=EDGE_LOOP('',(#7404));
#1665=EDGE_LOOP('',(#7405));
#1666=EDGE_LOOP('',(#7406,#7407,#7408,#7409));
#1667=EDGE_LOOP('',(#7410,#7411,#7412,#7413));
#1668=EDGE_LOOP('',(#7414,#7415,#7416,#7417));
#1669=EDGE_LOOP('',(#7418,#7419,#7420,#7421));
#1670=EDGE_LOOP('',(#7422,#7423,#7424,#7425));
#1671=EDGE_LOOP('',(#7426,#7427,#7428,#7429));
#1672=EDGE_LOOP('',(#7430,#7431,#7432,#7433));
#1673=EDGE_LOOP('',(#7434,#7435,#7436,#7437));
#1674=EDGE_LOOP('',(#7438,#7439,#7440,#7441));
#1675=EDGE_LOOP('',(#7442,#7443,#7444,#7445));
#1676=EDGE_LOOP('',(#7446,#7447,#7448,#7449));
#1677=EDGE_LOOP('',(#7450,#7451,#7452,#7453));
#1678=EDGE_LOOP('',(#7454,#7455,#7456,#7457));
#1679=EDGE_LOOP('',(#7458,#7459,#7460,#7461));
#1680=EDGE_LOOP('',(#7462));
#1681=EDGE_LOOP('',(#7463));
#1682=EDGE_LOOP('',(#7464));
#1683=EDGE_LOOP('',(#7465));
#1684=EDGE_LOOP('',(#7466,#7467,#7468,#7469));
#1685=EDGE_LOOP('',(#7470,#7471,#7472,#7473));
#1686=EDGE_LOOP('',(#7474));
#1687=EDGE_LOOP('',(#7475));
#1688=EDGE_LOOP('',(#7476));
#1689=EDGE_LOOP('',(#7477));
#1690=EDGE_LOOP('',(#7478,#7479,#7480,#7481));
#1691=EDGE_LOOP('',(#7482,#7483,#7484,#7485));
#1692=EDGE_LOOP('',(#7486));
#1693=EDGE_LOOP('',(#7487));
#1694=EDGE_LOOP('',(#7488));
#1695=EDGE_LOOP('',(#7489));
#1696=EDGE_LOOP('',(#7490,#7491,#7492,#7493));
#1697=EDGE_LOOP('',(#7494,#7495,#7496,#7497));
#1698=EDGE_LOOP('',(#7498));
#1699=EDGE_LOOP('',(#7499));
#1700=EDGE_LOOP('',(#7500));
#1701=EDGE_LOOP('',(#7501));
#1702=EDGE_LOOP('',(#7502,#7503,#7504,#7505));
#1703=EDGE_LOOP('',(#7506,#7507,#7508,#7509));
#1704=EDGE_LOOP('',(#7510,#7511,#7512,#7513));
#1705=EDGE_LOOP('',(#7514,#7515,#7516,#7517));
#1706=EDGE_LOOP('',(#7518,#7519,#7520,#7521));
#1707=EDGE_LOOP('',(#7522,#7523,#7524,#7525));
#1708=EDGE_LOOP('',(#7526,#7527,#7528,#7529));
#1709=EDGE_LOOP('',(#7530,#7531,#7532,#7533));
#1710=EDGE_LOOP('',(#7534));
#1711=EDGE_LOOP('',(#7535));
#1712=EDGE_LOOP('',(#7536,#7537,#7538,#7539));
#1713=EDGE_LOOP('',(#7540,#7541,#7542,#7543));
#1714=EDGE_LOOP('',(#7544));
#1715=EDGE_LOOP('',(#7545));
#1716=EDGE_LOOP('',(#7546));
#1717=EDGE_LOOP('',(#7547));
#1718=EDGE_LOOP('',(#7548));
#1719=EDGE_LOOP('',(#7549,#7550,#7551,#7552,#7553,#7554));
#1720=EDGE_LOOP('',(#7555,#7556,#7557,#7558,#7559,#7560));
#1721=EDGE_LOOP('',(#7561,#7562,#7563,#7564));
#1722=EDGE_LOOP('',(#7565));
#1723=EDGE_LOOP('',(#7566));
#1724=EDGE_LOOP('',(#7567));
#1725=EDGE_LOOP('',(#7568));
#1726=EDGE_LOOP('',(#7569));
#1727=EDGE_LOOP('',(#7570,#7571,#7572,#7573));
#1728=EDGE_LOOP('',(#7574,#7575,#7576,#7577));
#1729=EDGE_LOOP('',(#7578));
#1730=EDGE_LOOP('',(#7579));
#1731=EDGE_LOOP('',(#7580,#7581,#7582,#7583));
#1732=EDGE_LOOP('',(#7584));
#1733=EDGE_LOOP('',(#7585,#7586,#7587,#7588));
#1734=EDGE_LOOP('',(#7589));
#1735=EDGE_LOOP('',(#7590,#7591,#7592,#7593));
#1736=EDGE_LOOP('',(#7594));
#1737=EDGE_LOOP('',(#7595,#7596,#7597,#7598));
#1738=EDGE_LOOP('',(#7599));
#1739=EDGE_LOOP('',(#7600,#7601,#7602,#7603));
#1740=EDGE_LOOP('',(#7604));
#1741=EDGE_LOOP('',(#7605));
#1742=EDGE_LOOP('',(#7606,#7607,#7608,#7609));
#1743=EDGE_LOOP('',(#7610,#7611,#7612,#7613));
#1744=EDGE_LOOP('',(#7614));
#1745=EDGE_LOOP('',(#7615));
#1746=EDGE_LOOP('',(#7616));
#1747=EDGE_LOOP('',(#7617));
#1748=EDGE_LOOP('',(#7618));
#1749=EDGE_LOOP('',(#7619,#7620,#7621,#7622));
#1750=EDGE_LOOP('',(#7623,#7624,#7625,#7626));
#1751=EDGE_LOOP('',(#7627));
#1752=EDGE_LOOP('',(#7628,#7629,#7630,#7631));
#1753=EDGE_LOOP('',(#7632,#7633,#7634,#7635));
#1754=EDGE_LOOP('',(#7636,#7637,#7638,#7639));
#1755=EDGE_LOOP('',(#7640,#7641,#7642,#7643));
#1756=EDGE_LOOP('',(#7644,#7645,#7646,#7647));
#1757=EDGE_LOOP('',(#7648,#7649,#7650,#7651));
#1758=EDGE_LOOP('',(#7652,#7653,#7654,#7655));
#1759=EDGE_LOOP('',(#7656,#7657,#7658,#7659));
#1760=EDGE_LOOP('',(#7660,#7661,#7662,#7663));
#1761=EDGE_LOOP('',(#7664,#7665,#7666,#7667,#7668,#7669));
#1762=EDGE_LOOP('',(#7670));
#1763=EDGE_LOOP('',(#7671));
#1764=EDGE_LOOP('',(#7672,#7673,#7674,#7675));
#1765=EDGE_LOOP('',(#7676));
#1766=EDGE_LOOP('',(#7677,#7678,#7679,#7680,#7681,#7682));
#1767=EDGE_LOOP('',(#7683,#7684,#7685,#7686));
#1768=EDGE_LOOP('',(#7687));
#1769=EDGE_LOOP('',(#7688,#7689,#7690,#7691));
#1770=EDGE_LOOP('',(#7692,#7693,#7694,#7695));
#1771=EDGE_LOOP('',(#7696,#7697,#7698,#7699));
#1772=EDGE_LOOP('',(#7700,#7701,#7702,#7703));
#1773=EDGE_LOOP('',(#7704,#7705,#7706,#7707));
#1774=EDGE_LOOP('',(#7708,#7709,#7710,#7711));
#1775=EDGE_LOOP('',(#7712,#7713,#7714,#7715,#7716,#7717));
#1776=EDGE_LOOP('',(#7718));
#1777=EDGE_LOOP('',(#7719));
#1778=EDGE_LOOP('',(#7720,#7721,#7722,#7723));
#1779=EDGE_LOOP('',(#7724));
#1780=EDGE_LOOP('',(#7725,#7726,#7727,#7728,#7729,#7730));
#1781=EDGE_LOOP('',(#7731,#7732,#7733,#7734));
#1782=EDGE_LOOP('',(#7735));
#1783=EDGE_LOOP('',(#7736,#7737,#7738,#7739));
#1784=EDGE_LOOP('',(#7740,#7741,#7742,#7743));
#1785=EDGE_LOOP('',(#7744,#7745,#7746,#7747));
#1786=EDGE_LOOP('',(#7748,#7749,#7750,#7751));
#1787=EDGE_LOOP('',(#7752,#7753,#7754,#7755));
#1788=EDGE_LOOP('',(#7756,#7757,#7758,#7759));
#1789=EDGE_LOOP('',(#7760,#7761,#7762,#7763,#7764,#7765));
#1790=EDGE_LOOP('',(#7766));
#1791=EDGE_LOOP('',(#7767));
#1792=EDGE_LOOP('',(#7768,#7769,#7770,#7771));
#1793=EDGE_LOOP('',(#7772));
#1794=EDGE_LOOP('',(#7773,#7774,#7775,#7776,#7777,#7778));
#1795=EDGE_LOOP('',(#7779,#7780,#7781,#7782));
#1796=EDGE_LOOP('',(#7783));
#1797=EDGE_LOOP('',(#7784,#7785,#7786,#7787));
#1798=EDGE_LOOP('',(#7788,#7789,#7790,#7791));
#1799=EDGE_LOOP('',(#7792,#7793,#7794,#7795));
#1800=EDGE_LOOP('',(#7796,#7797,#7798,#7799));
#1801=EDGE_LOOP('',(#7800,#7801,#7802,#7803));
#1802=EDGE_LOOP('',(#7804,#7805,#7806,#7807));
#1803=EDGE_LOOP('',(#7808,#7809,#7810,#7811,#7812,#7813));
#1804=EDGE_LOOP('',(#7814));
#1805=EDGE_LOOP('',(#7815));
#1806=EDGE_LOOP('',(#7816,#7817,#7818,#7819));
#1807=EDGE_LOOP('',(#7820));
#1808=EDGE_LOOP('',(#7821,#7822,#7823,#7824,#7825,#7826));
#1809=EDGE_LOOP('',(#7827,#7828,#7829,#7830));
#1810=EDGE_LOOP('',(#7831));
#1811=EDGE_LOOP('',(#7832,#7833));
#1812=EDGE_LOOP('',(#7834,#7835,#7836,#7837,#7838,#7839,#7840,#7841));
#1813=EDGE_LOOP('',(#7842,#7843,#7844,#7845,#7846,#7847,#7848,#7849));
#1814=EDGE_LOOP('',(#7850,#7851));
#1815=EDGE_LOOP('',(#7852,#7853,#7854,#7855,#7856));
#1816=EDGE_LOOP('',(#7857,#7858));
#1817=EDGE_LOOP('',(#7859));
#1818=EDGE_LOOP('',(#7860));
#1819=EDGE_LOOP('',(#7861,#7862,#7863));
#1820=EDGE_LOOP('',(#7864,#7865,#7866));
#1821=EDGE_LOOP('',(#7867,#7868,#7869));
#1822=EDGE_LOOP('',(#7870,#7871,#7872,#7873));
#1823=EDGE_LOOP('',(#7874,#7875,#7876));
#1824=EDGE_LOOP('',(#7877,#7878,#7879,#7880));
#1825=EDGE_LOOP('',(#7881,#7882,#7883,#7884));
#1826=EDGE_LOOP('',(#7885,#7886,#7887,#7888,#7889,#7890,#7891,#7892,#7893,
#7894,#7895,#7896,#7897,#7898,#7899,#7900,#7901,#7902,#7903,#7904));
#1827=EDGE_LOOP('',(#7905));
#1828=EDGE_LOOP('',(#7906));
#1829=EDGE_LOOP('',(#7907,#7908,#7909,#7910));
#1830=EDGE_LOOP('',(#7911,#7912,#7913,#7914,#7915,#7916,#7917,#7918,#7919,
#7920,#7921,#7922));
#1831=EDGE_LOOP('',(#7923,#7924,#7925,#7926,#7927));
#1832=EDGE_LOOP('',(#7928,#7929,#7930,#7931,#7932,#7933));
#1833=EDGE_LOOP('',(#7934,#7935,#7936,#7937));
#1834=EDGE_LOOP('',(#7938,#7939,#7940,#7941));
#1835=EDGE_LOOP('',(#7942,#7943,#7944,#7945,#7946,#7947));
#1836=EDGE_LOOP('',(#7948,#7949,#7950,#7951));
#1837=EDGE_LOOP('',(#7952,#7953,#7954,#7955));
#1838=EDGE_LOOP('',(#7956,#7957,#7958,#7959));
#1839=EDGE_LOOP('',(#7960,#7961,#7962,#7963));
#1840=EDGE_LOOP('',(#7964,#7965,#7966,#7967));
#1841=EDGE_LOOP('',(#7968,#7969,#7970,#7971));
#1842=EDGE_LOOP('',(#7972,#7973,#7974,#7975));
#1843=EDGE_LOOP('',(#7976,#7977,#7978,#7979));
#1844=EDGE_LOOP('',(#7980,#7981,#7982,#7983));
#1845=EDGE_LOOP('',(#7984,#7985,#7986,#7987));
#1846=EDGE_LOOP('',(#7988));
#1847=EDGE_LOOP('',(#7989));
#1848=EDGE_LOOP('',(#7990,#7991,#7992,#7993));
#1849=EDGE_LOOP('',(#7994));
#1850=EDGE_LOOP('',(#7995));
#1851=EDGE_LOOP('',(#7996,#7997));
#1852=EDGE_LOOP('',(#7998));
#1853=EDGE_LOOP('',(#7999));
#1854=EDGE_LOOP('',(#8000));
#1855=EDGE_LOOP('',(#8001));
#1856=EDGE_LOOP('',(#8002,#8003,#8004,#8005,#8006,#8007));
#1857=EDGE_LOOP('',(#8008,#8009,#8010,#8011,#8012,#8013));
#1858=EDGE_LOOP('',(#8014,#8015,#8016,#8017));
#1859=EDGE_LOOP('',(#8018,#8019,#8020));
#1860=EDGE_LOOP('',(#8021,#8022,#8023));
#1861=EDGE_LOOP('',(#8024,#8025,#8026));
#1862=EDGE_LOOP('',(#8027,#8028,#8029));
#1863=EDGE_LOOP('',(#8030,#8031,#8032));
#1864=EDGE_LOOP('',(#8033,#8034,#8035));
#1865=EDGE_LOOP('',(#8036,#8037,#8038,#8039,#8040,#8041));
#1866=EDGE_LOOP('',(#8042,#8043,#8044,#8045,#8046,#8047));
#1867=EDGE_LOOP('',(#8048,#8049,#8050,#8051,#8052,#8053));
#1868=EDGE_LOOP('',(#8054,#8055,#8056,#8057,#8058,#8059));
#1869=EDGE_LOOP('',(#8060));
#1870=EDGE_LOOP('',(#8061));
#1871=EDGE_LOOP('',(#8062));
#1872=EDGE_LOOP('',(#8063));
#1873=EDGE_LOOP('',(#8064,#8065,#8066,#8067));
#1874=EDGE_LOOP('',(#8068));
#1875=EDGE_LOOP('',(#8069));
#1876=EDGE_LOOP('',(#8070,#8071,#8072,#8073));
#1877=EDGE_LOOP('',(#8074));
#1878=EDGE_LOOP('',(#8075));
#1879=EDGE_LOOP('',(#8076));
#1880=EDGE_LOOP('',(#8077));
#1881=EDGE_LOOP('',(#8078));
#1882=EDGE_LOOP('',(#8079));
#1883=EDGE_LOOP('',(#8080,#8081,#8082,#8083));
#1884=EDGE_LOOP('',(#8084,#8085,#8086,#8087));
#1885=EDGE_LOOP('',(#8088));
#1886=EDGE_LOOP('',(#8089));
#1887=EDGE_LOOP('',(#8090));
#1888=EDGE_LOOP('',(#8091));
#1889=EDGE_LOOP('',(#8092,#8093,#8094,#8095));
#1890=EDGE_LOOP('',(#8096,#8097,#8098,#8099));
#1891=EDGE_LOOP('',(#8100,#8101,#8102,#8103));
#1892=EDGE_LOOP('',(#8104,#8105,#8106,#8107));
#1893=EDGE_LOOP('',(#8108,#8109,#8110,#8111));
#1894=EDGE_LOOP('',(#8112,#8113,#8114,#8115));
#1895=EDGE_LOOP('',(#8116,#8117,#8118,#8119,#8120,#8121));
#1896=EDGE_LOOP('',(#8122,#8123,#8124,#8125,#8126,#8127));
#1897=EDGE_LOOP('',(#8128));
#1898=EDGE_LOOP('',(#8129));
#1899=EDGE_LOOP('',(#8130,#8131,#8132,#8133));
#1900=EDGE_LOOP('',(#8134,#8135,#8136,#8137));
#1901=EDGE_LOOP('',(#8138,#8139,#8140,#8141));
#1902=EDGE_LOOP('',(#8142));
#1903=EDGE_LOOP('',(#8143));
#1904=EDGE_LOOP('',(#8144,#8145,#8146,#8147));
#1905=EDGE_LOOP('',(#8148,#8149,#8150,#8151));
#1906=EDGE_LOOP('',(#8152,#8153,#8154,#8155));
#1907=EDGE_LOOP('',(#8156,#8157,#8158,#8159));
#1908=EDGE_LOOP('',(#8160,#8161,#8162,#8163));
#1909=EDGE_LOOP('',(#8164,#8165,#8166,#8167));
#1910=EDGE_LOOP('',(#8168,#8169,#8170,#8171));
#1911=EDGE_LOOP('',(#8172,#8173,#8174,#8175));
#1912=EDGE_LOOP('',(#8176,#8177,#8178,#8179,#8180,#8181));
#1913=EDGE_LOOP('',(#8182,#8183,#8184,#8185,#8186,#8187));
#1914=EDGE_LOOP('',(#8188));
#1915=EDGE_LOOP('',(#8189));
#1916=EDGE_LOOP('',(#8190,#8191,#8192,#8193));
#1917=EDGE_LOOP('',(#8194,#8195,#8196,#8197));
#1918=EDGE_LOOP('',(#8198,#8199,#8200,#8201));
#1919=EDGE_LOOP('',(#8202));
#1920=EDGE_LOOP('',(#8203));
#1921=EDGE_LOOP('',(#8204,#8205,#8206,#8207));
#1922=EDGE_LOOP('',(#8208,#8209,#8210,#8211));
#1923=EDGE_LOOP('',(#8212,#8213,#8214,#8215));
#1924=EDGE_LOOP('',(#8216,#8217,#8218,#8219));
#1925=EDGE_LOOP('',(#8220,#8221,#8222,#8223));
#1926=EDGE_LOOP('',(#8224,#8225,#8226,#8227));
#1927=EDGE_LOOP('',(#8228,#8229,#8230,#8231));
#1928=EDGE_LOOP('',(#8232,#8233,#8234,#8235));
#1929=EDGE_LOOP('',(#8236));
#1930=EDGE_LOOP('',(#8237,#8238,#8239,#8240));
#1931=EDGE_LOOP('',(#8241,#8242,#8243,#8244));
#1932=EDGE_LOOP('',(#8245));
#1933=EDGE_LOOP('',(#8246));
#1934=EDGE_LOOP('',(#8247));
#1935=EDGE_LOOP('',(#8248,#8249,#8250,#8251));
#1936=EDGE_LOOP('',(#8252));
#1937=EDGE_LOOP('',(#8253));
#1938=EDGE_LOOP('',(#8254,#8255));
#1939=EDGE_LOOP('',(#8256,#8257,#8258,#8259,#8260,#8261,#8262,#8263,#8264));
#1940=EDGE_LOOP('',(#8265,#8266,#8267));
#1941=EDGE_LOOP('',(#8268,#8269,#8270,#8271));
#1942=EDGE_LOOP('',(#8272,#8273,#8274,#8275));
#1943=EDGE_LOOP('',(#8276,#8277,#8278,#8279));
#1944=EDGE_LOOP('',(#8280,#8281));
#1945=EDGE_LOOP('',(#8282));
#1946=EDGE_LOOP('',(#8283));
#1947=EDGE_LOOP('',(#8284));
#1948=EDGE_LOOP('',(#8285));
#1949=EDGE_LOOP('',(#8286,#8287));
#1950=EDGE_LOOP('',(#8288,#8289,#8290,#8291,#8292,#8293,#8294,#8295,#8296));
#1951=EDGE_LOOP('',(#8297,#8298,#8299));
#1952=EDGE_LOOP('',(#8300,#8301,#8302,#8303));
#1953=EDGE_LOOP('',(#8304,#8305,#8306,#8307));
#1954=EDGE_LOOP('',(#8308,#8309,#8310,#8311));
#1955=EDGE_LOOP('',(#8312));
#1956=EDGE_LOOP('',(#8313,#8314,#8315,#8316));
#1957=EDGE_LOOP('',(#8317,#8318,#8319,#8320));
#1958=EDGE_LOOP('',(#8321,#8322,#8323,#8324));
#1959=EDGE_LOOP('',(#8325));
#1960=EDGE_LOOP('',(#8326));
#1961=EDGE_LOOP('',(#8327));
#1962=EDGE_LOOP('',(#8328));
#1963=EDGE_LOOP('',(#8329,#8330,#8331,#8332));
#1964=EDGE_LOOP('',(#8333,#8334,#8335,#8336));
#1965=EDGE_LOOP('',(#8337,#8338));
#1966=EDGE_LOOP('',(#8339,#8340,#8341,#8342));
#1967=EDGE_LOOP('',(#8343));
#1968=EDGE_LOOP('',(#8344,#8345,#8346,#8347));
#1969=EDGE_LOOP('',(#8348,#8349));
#1970=EDGE_LOOP('',(#8350,#8351,#8352,#8353,#8354,#8355,#8356,#8357,#8358));
#1971=EDGE_LOOP('',(#8359,#8360,#8361));
#1972=EDGE_LOOP('',(#8362,#8363,#8364,#8365));
#1973=EDGE_LOOP('',(#8366,#8367,#8368,#8369));
#1974=EDGE_LOOP('',(#8370,#8371,#8372,#8373));
#1975=EDGE_LOOP('',(#8374,#8375));
#1976=EDGE_LOOP('',(#8376));
#1977=EDGE_LOOP('',(#8377));
#1978=EDGE_LOOP('',(#8378));
#1979=EDGE_LOOP('',(#8379));
#1980=EDGE_LOOP('',(#8380,#8381));
#1981=EDGE_LOOP('',(#8382,#8383,#8384,#8385,#8386,#8387,#8388,#8389,#8390));
#1982=EDGE_LOOP('',(#8391,#8392,#8393));
#1983=EDGE_LOOP('',(#8394,#8395,#8396,#8397));
#1984=EDGE_LOOP('',(#8398,#8399,#8400,#8401));
#1985=EDGE_LOOP('',(#8402,#8403,#8404,#8405));
#1986=EDGE_LOOP('',(#8406,#8407));
#1987=EDGE_LOOP('',(#8408));
#1988=EDGE_LOOP('',(#8409));
#1989=EDGE_LOOP('',(#8410));
#1990=EDGE_LOOP('',(#8411));
#1991=EDGE_LOOP('',(#8412,#8413,#8414,#8415));
#1992=EDGE_LOOP('',(#8416,#8417,#8418,#8419));
#1993=EDGE_LOOP('',(#8420));
#1994=EDGE_LOOP('',(#8421));
#1995=EDGE_LOOP('',(#8422));
#1996=EDGE_LOOP('',(#8423));
#1997=EDGE_LOOP('',(#8424,#8425,#8426,#8427));
#1998=EDGE_LOOP('',(#8428,#8429,#8430,#8431));
#1999=EDGE_LOOP('',(#8432,#8433,#8434,#8435));
#2000=EDGE_LOOP('',(#8436,#8437,#8438,#8439));
#2001=EDGE_LOOP('',(#8440,#8441,#8442,#8443));
#2002=EDGE_LOOP('',(#8444,#8445,#8446,#8447));
#2003=EDGE_LOOP('',(#8448,#8449,#8450,#8451,#8452,#8453));
#2004=EDGE_LOOP('',(#8454));
#2005=EDGE_LOOP('',(#8455,#8456,#8457,#8458,#8459,#8460));
#2006=EDGE_LOOP('',(#8461,#8462,#8463,#8464));
#2007=EDGE_LOOP('',(#8465,#8466,#8467,#8468));
#2008=EDGE_LOOP('',(#8469,#8470,#8471,#8472));
#2009=EDGE_LOOP('',(#8473));
#2010=EDGE_LOOP('',(#8474,#8475,#8476,#8477,#8478));
#2011=EDGE_LOOP('',(#8479,#8480,#8481,#8482));
#2012=EDGE_LOOP('',(#8483,#8484));
#2013=EDGE_LOOP('',(#8485,#8486,#8487,#8488));
#2014=EDGE_LOOP('',(#8489,#8490,#8491,#8492));
#2015=EDGE_LOOP('',(#8493,#8494,#8495,#8496));
#2016=EDGE_LOOP('',(#8497,#8498,#8499,#8500));
#2017=EDGE_LOOP('',(#8501,#8502,#8503,#8504));
#2018=EDGE_LOOP('',(#8505,#8506,#8507,#8508));
#2019=EDGE_LOOP('',(#8509,#8510,#8511,#8512));
#2020=EDGE_LOOP('',(#8513,#8514,#8515,#8516));
#2021=EDGE_LOOP('',(#8517,#8518,#8519,#8520));
#2022=EDGE_LOOP('',(#8521,#8522,#8523,#8524));
#2023=EDGE_LOOP('',(#8525,#8526,#8527,#8528));
#2024=EDGE_LOOP('',(#8529,#8530,#8531,#8532));
#2025=EDGE_LOOP('',(#8533,#8534,#8535,#8536));
#2026=EDGE_LOOP('',(#8537,#8538,#8539,#8540));
#2027=EDGE_LOOP('',(#8541,#8542,#8543,#8544));
#2028=EDGE_LOOP('',(#8545,#8546,#8547,#8548));
#2029=EDGE_LOOP('',(#8549,#8550,#8551,#8552));
#2030=EDGE_LOOP('',(#8553,#8554,#8555,#8556));
#2031=EDGE_LOOP('',(#8557,#8558,#8559,#8560,#8561,#8562,#8563,#8564,#8565,
#8566,#8567,#8568,#8569,#8570,#8571,#8572,#8573,#8574));
#2032=EDGE_LOOP('',(#8575,#8576));
#2033=EDGE_LOOP('',(#8577,#8578));
#2034=EDGE_LOOP('',(#8579,#8580));
#2035=EDGE_LOOP('',(#8581,#8582));
#2036=EDGE_LOOP('',(#8583,#8584));
#2037=EDGE_LOOP('',(#8585,#8586));
#2038=EDGE_LOOP('',(#8587,#8588));
#2039=EDGE_LOOP('',(#8589,#8590));
#2040=EDGE_LOOP('',(#8591,#8592,#8593,#8594,#8595,#8596,#8597,#8598,#8599,
#8600,#8601,#8602,#8603,#8604,#8605,#8606,#8607,#8608,#8609,#8610,#8611,
#8612,#8613,#8614,#8615,#8616,#8617,#8618,#8619,#8620,#8621,#8622,#8623,
#8624));
#2041=EDGE_LOOP('',(#8625));
#2042=EDGE_LOOP('',(#8626,#8627,#8628,#8629));
#2043=EDGE_LOOP('',(#8630,#8631,#8632,#8633));
#2044=EDGE_LOOP('',(#8634,#8635,#8636,#8637));
#2045=EDGE_LOOP('',(#8638,#8639,#8640,#8641));
#2046=EDGE_LOOP('',(#8642,#8643,#8644,#8645));
#2047=EDGE_LOOP('',(#8646,#8647,#8648,#8649));
#2048=EDGE_LOOP('',(#8650,#8651,#8652,#8653));
#2049=EDGE_LOOP('',(#8654,#8655,#8656,#8657));
#2050=EDGE_LOOP('',(#8658,#8659,#8660,#8661));
#2051=EDGE_LOOP('',(#8662,#8663,#8664,#8665));
#2052=EDGE_LOOP('',(#8666,#8667,#8668,#8669));
#2053=EDGE_LOOP('',(#8670,#8671,#8672,#8673));
#2054=EDGE_LOOP('',(#8674,#8675,#8676,#8677));
#2055=EDGE_LOOP('',(#8678,#8679,#8680,#8681));
#2056=EDGE_LOOP('',(#8682,#8683,#8684,#8685));
#2057=EDGE_LOOP('',(#8686,#8687,#8688,#8689));
#2058=EDGE_LOOP('',(#8690,#8691,#8692,#8693));
#2059=EDGE_LOOP('',(#8694,#8695,#8696,#8697));
#2060=EDGE_LOOP('',(#8698,#8699,#8700,#8701,#8702,#8703,#8704,#8705,#8706,
#8707,#8708,#8709,#8710,#8711,#8712,#8713,#8714,#8715));
#2061=EDGE_LOOP('',(#8716,#8717));
#2062=EDGE_LOOP('',(#8718,#8719));
#2063=EDGE_LOOP('',(#8720,#8721));
#2064=EDGE_LOOP('',(#8722,#8723));
#2065=EDGE_LOOP('',(#8724,#8725));
#2066=EDGE_LOOP('',(#8726,#8727));
#2067=EDGE_LOOP('',(#8728,#8729));
#2068=EDGE_LOOP('',(#8730,#8731));
#2069=EDGE_LOOP('',(#8732,#8733,#8734,#8735));
#2070=EDGE_LOOP('',(#8736,#8737,#8738,#8739));
#2071=EDGE_LOOP('',(#8740,#8741,#8742,#8743));
#2072=EDGE_LOOP('',(#8744,#8745,#8746,#8747));
#2073=EDGE_LOOP('',(#8748,#8749,#8750,#8751));
#2074=EDGE_LOOP('',(#8752,#8753,#8754,#8755));
#2075=EDGE_LOOP('',(#8756,#8757,#8758,#8759));
#2076=EDGE_LOOP('',(#8760,#8761,#8762,#8763));
#2077=EDGE_LOOP('',(#8764,#8765,#8766,#8767));
#2078=EDGE_LOOP('',(#8768,#8769,#8770,#8771));
#2079=EDGE_LOOP('',(#8772,#8773,#8774,#8775));
#2080=EDGE_LOOP('',(#8776,#8777,#8778,#8779));
#2081=EDGE_LOOP('',(#8780,#8781,#8782,#8783));
#2082=EDGE_LOOP('',(#8784,#8785,#8786,#8787));
#2083=EDGE_LOOP('',(#8788,#8789,#8790,#8791));
#2084=EDGE_LOOP('',(#8792,#8793,#8794,#8795));
#2085=EDGE_LOOP('',(#8796,#8797,#8798,#8799));
#2086=EDGE_LOOP('',(#8800,#8801,#8802,#8803));
#2087=EDGE_LOOP('',(#8804,#8805,#8806,#8807,#8808,#8809,#8810,#8811,#8812,
#8813,#8814,#8815,#8816,#8817,#8818,#8819,#8820,#8821));
#2088=EDGE_LOOP('',(#8822,#8823));
#2089=EDGE_LOOP('',(#8824,#8825));
#2090=EDGE_LOOP('',(#8826,#8827));
#2091=EDGE_LOOP('',(#8828,#8829));
#2092=EDGE_LOOP('',(#8830,#8831));
#2093=EDGE_LOOP('',(#8832,#8833));
#2094=EDGE_LOOP('',(#8834,#8835));
#2095=EDGE_LOOP('',(#8836,#8837));
#2096=EDGE_LOOP('',(#8838,#8839,#8840,#8841,#8842,#8843,#8844,#8845,#8846,
#8847,#8848,#8849,#8850,#8851,#8852,#8853,#8854,#8855,#8856,#8857,#8858,
#8859,#8860,#8861,#8862,#8863,#8864,#8865,#8866,#8867,#8868));
#2097=EDGE_LOOP('',(#8869));
#2098=EDGE_LOOP('',(#8870));
#2099=EDGE_LOOP('',(#8871));
#2100=EDGE_LOOP('',(#8872,#8873,#8874,#8875,#8876,#8877));
#2101=EDGE_LOOP('',(#8878,#8879,#8880,#8881));
#2102=EDGE_LOOP('',(#8882,#8883));
#2103=EDGE_LOOP('',(#8884,#8885,#8886,#8887));
#2104=EDGE_LOOP('',(#8888,#8889,#8890,#8891));
#2105=EDGE_LOOP('',(#8892,#8893,#8894,#8895));
#2106=EDGE_LOOP('',(#8896,#8897,#8898,#8899));
#2107=EDGE_LOOP('',(#8900,#8901,#8902,#8903));
#2108=EDGE_LOOP('',(#8904,#8905,#8906,#8907));
#2109=EDGE_LOOP('',(#8908,#8909,#8910,#8911));
#2110=EDGE_LOOP('',(#8912,#8913,#8914,#8915));
#2111=EDGE_LOOP('',(#8916,#8917,#8918,#8919));
#2112=EDGE_LOOP('',(#8920,#8921,#8922,#8923));
#2113=EDGE_LOOP('',(#8924,#8925,#8926,#8927));
#2114=EDGE_LOOP('',(#8928,#8929,#8930,#8931));
#2115=EDGE_LOOP('',(#8932,#8933,#8934,#8935));
#2116=EDGE_LOOP('',(#8936,#8937,#8938,#8939));
#2117=EDGE_LOOP('',(#8940,#8941,#8942,#8943));
#2118=EDGE_LOOP('',(#8944,#8945,#8946,#8947));
#2119=EDGE_LOOP('',(#8948,#8949,#8950,#8951));
#2120=EDGE_LOOP('',(#8952,#8953,#8954,#8955));
#2121=EDGE_LOOP('',(#8956,#8957,#8958,#8959,#8960,#8961,#8962,#8963,#8964,
#8965,#8966,#8967,#8968,#8969,#8970,#8971,#8972,#8973));
#2122=EDGE_LOOP('',(#8974,#8975));
#2123=EDGE_LOOP('',(#8976,#8977));
#2124=EDGE_LOOP('',(#8978,#8979));
#2125=EDGE_LOOP('',(#8980,#8981));
#2126=EDGE_LOOP('',(#8982,#8983));
#2127=EDGE_LOOP('',(#8984,#8985));
#2128=EDGE_LOOP('',(#8986,#8987,#8988,#8989,#8990,#8991,#8992,#8993,#8994,
#8995,#8996,#8997,#8998,#8999,#9000,#9001,#9002,#9003,#9004,#9005,#9006,
#9007,#9008,#9009,#9010,#9011,#9012,#9013,#9014,#9015,#9016,#9017,#9018,
#9019));
#2129=EDGE_LOOP('',(#9020));
#2130=EDGE_LOOP('',(#9021,#9022));
#2131=EDGE_LOOP('',(#9023,#9024));
#2132=EDGE_LOOP('',(#9025,#9026,#9027,#9028));
#2133=EDGE_LOOP('',(#9029,#9030,#9031,#9032));
#2134=EDGE_LOOP('',(#9033,#9034,#9035,#9036));
#2135=EDGE_LOOP('',(#9037,#9038,#9039,#9040));
#2136=EDGE_LOOP('',(#9041,#9042,#9043,#9044));
#2137=EDGE_LOOP('',(#9045,#9046,#9047,#9048));
#2138=EDGE_LOOP('',(#9049,#9050,#9051,#9052));
#2139=EDGE_LOOP('',(#9053,#9054,#9055,#9056));
#2140=EDGE_LOOP('',(#9057,#9058,#9059,#9060));
#2141=EDGE_LOOP('',(#9061,#9062,#9063,#9064));
#2142=EDGE_LOOP('',(#9065,#9066,#9067,#9068));
#2143=EDGE_LOOP('',(#9069,#9070,#9071,#9072));
#2144=EDGE_LOOP('',(#9073,#9074,#9075,#9076));
#2145=EDGE_LOOP('',(#9077,#9078,#9079,#9080));
#2146=EDGE_LOOP('',(#9081,#9082,#9083,#9084));
#2147=EDGE_LOOP('',(#9085,#9086,#9087,#9088));
#2148=EDGE_LOOP('',(#9089,#9090,#9091,#9092));
#2149=EDGE_LOOP('',(#9093,#9094,#9095,#9096));
#2150=EDGE_LOOP('',(#9097,#9098,#9099,#9100,#9101,#9102,#9103,#9104,#9105,
#9106,#9107,#9108,#9109,#9110,#9111,#9112,#9113,#9114));
#2151=EDGE_LOOP('',(#9115,#9116));
#2152=EDGE_LOOP('',(#9117,#9118));
#2153=EDGE_LOOP('',(#9119,#9120));
#2154=EDGE_LOOP('',(#9121,#9122));
#2155=EDGE_LOOP('',(#9123,#9124));
#2156=EDGE_LOOP('',(#9125,#9126));
#2157=EDGE_LOOP('',(#9127,#9128));
#2158=EDGE_LOOP('',(#9129,#9130));
#2159=EDGE_LOOP('',(#9131,#9132,#9133,#9134));
#2160=EDGE_LOOP('',(#9135,#9136,#9137,#9138));
#2161=EDGE_LOOP('',(#9139,#9140,#9141,#9142));
#2162=EDGE_LOOP('',(#9143,#9144,#9145,#9146));
#2163=EDGE_LOOP('',(#9147,#9148,#9149,#9150));
#2164=EDGE_LOOP('',(#9151,#9152,#9153,#9154));
#2165=EDGE_LOOP('',(#9155,#9156,#9157,#9158));
#2166=EDGE_LOOP('',(#9159,#9160,#9161,#9162));
#2167=EDGE_LOOP('',(#9163,#9164,#9165,#9166));
#2168=EDGE_LOOP('',(#9167,#9168,#9169,#9170));
#2169=EDGE_LOOP('',(#9171,#9172,#9173,#9174));
#2170=EDGE_LOOP('',(#9175,#9176,#9177,#9178));
#2171=EDGE_LOOP('',(#9179,#9180,#9181,#9182));
#2172=EDGE_LOOP('',(#9183,#9184,#9185,#9186));
#2173=EDGE_LOOP('',(#9187,#9188,#9189,#9190));
#2174=EDGE_LOOP('',(#9191,#9192,#9193,#9194));
#2175=EDGE_LOOP('',(#9195,#9196,#9197,#9198));
#2176=EDGE_LOOP('',(#9199,#9200,#9201,#9202));
#2177=EDGE_LOOP('',(#9203,#9204,#9205,#9206,#9207,#9208,#9209,#9210,#9211,
#9212,#9213,#9214,#9215,#9216,#9217,#9218,#9219,#9220));
#2178=EDGE_LOOP('',(#9221,#9222));
#2179=EDGE_LOOP('',(#9223,#9224));
#2180=EDGE_LOOP('',(#9225,#9226));
#2181=EDGE_LOOP('',(#9227,#9228));
#2182=EDGE_LOOP('',(#9229,#9230));
#2183=EDGE_LOOP('',(#9231,#9232));
#2184=EDGE_LOOP('',(#9233,#9234));
#2185=EDGE_LOOP('',(#9235,#9236));
#2186=EDGE_LOOP('',(#9237,#9238,#9239,#9240,#9241,#9242,#9243,#9244,#9245,
#9246,#9247,#9248,#9249,#9250,#9251,#9252,#9253,#9254,#9255,#9256,#9257,
#9258,#9259,#9260,#9261,#9262,#9263,#9264,#9265,#9266,#9267));
#2187=EDGE_LOOP('',(#9268,#9269));
#2188=EDGE_LOOP('',(#9270));
#2189=EDGE_LOOP('',(#9271));
#2190=EDGE_LOOP('',(#9272,#9273,#9274,#9275,#9276,#9277,#9278,#9279,#9280,
#9281,#9282,#9283,#9284,#9285,#9286,#9287,#9288,#9289,#9290,#9291,#9292,
#9293,#9294,#9295,#9296,#9297,#9298,#9299,#9300,#9301,#9302,#9303,#9304,
#9305,#9306,#9307,#9308,#9309,#9310,#9311,#9312,#9313,#9314,#9315,#9316,
#9317,#9318,#9319,#9320,#9321,#9322,#9323,#9324,#9325));
#2191=EDGE_LOOP('',(#9326,#9327,#9328,#9329));
#2192=EDGE_LOOP('',(#9330,#9331,#9332,#9333));
#2193=EDGE_LOOP('',(#9334,#9335,#9336,#9337));
#2194=EDGE_LOOP('',(#9338,#9339,#9340,#9341));
#2195=EDGE_LOOP('',(#9342,#9343,#9344,#9345));
#2196=EDGE_LOOP('',(#9346,#9347,#9348,#9349));
#2197=EDGE_LOOP('',(#9350,#9351,#9352,#9353,#9354,#9355,#9356,#9357,#9358,
#9359,#9360,#9361,#9362,#9363,#9364,#9365,#9366,#9367,#9368,#9369,#9370,
#9371,#9372,#9373,#9374,#9375,#9376,#9377,#9378,#9379,#9380,#9381,#9382,
#9383,#9384,#9385,#9386,#9387,#9388,#9389,#9390,#9391,#9392,#9393,#9394,
#9395,#9396,#9397,#9398,#9399,#9400,#9401,#9402,#9403));
#2198=EDGE_LOOP('',(#9404,#9405,#9406,#9407,#9408,#9409,#9410,#9411));
#2199=EDGE_LOOP('',(#9412,#9413,#9414,#9415));
#2200=EDGE_LOOP('',(#9416,#9417,#9418,#9419));
#2201=EDGE_LOOP('',(#9420,#9421,#9422,#9423));
#2202=EDGE_LOOP('',(#9424,#9425,#9426,#9427));
#2203=EDGE_LOOP('',(#9428,#9429,#9430,#9431));
#2204=EDGE_LOOP('',(#9432,#9433,#9434,#9435));
#2205=EDGE_LOOP('',(#9436,#9437,#9438,#9439));
#2206=EDGE_LOOP('',(#9440,#9441,#9442,#9443,#9444,#9445,#9446,#9447,#9448,
#9449,#9450,#9451,#9452,#9453));
#2207=EDGE_LOOP('',(#9454,#9455,#9456,#9457));
#2208=EDGE_LOOP('',(#9458,#9459,#9460,#9461));
#2209=EDGE_LOOP('',(#9462,#9463,#9464,#9465));
#2210=EDGE_LOOP('',(#9466,#9467,#9468,#9469));
#2211=EDGE_LOOP('',(#9470,#9471,#9472,#9473));
#2212=EDGE_LOOP('',(#9474,#9475,#9476,#9477));
#2213=EDGE_LOOP('',(#9478,#9479,#9480,#9481));
#2214=EDGE_LOOP('',(#9482,#9483,#9484,#9485));
#2215=EDGE_LOOP('',(#9486,#9487,#9488,#9489));
#2216=EDGE_LOOP('',(#9490,#9491,#9492,#9493));
#2217=EDGE_LOOP('',(#9494,#9495,#9496,#9497));
#2218=EDGE_LOOP('',(#9498,#9499,#9500,#9501,#9502,#9503,#9504,#9505));
#2219=EDGE_LOOP('',(#9506,#9507,#9508,#9509,#9510,#9511,#9512,#9513,#9514,
#9515,#9516,#9517,#9518,#9519));
#2220=EDGE_LOOP('',(#9520,#9521,#9522,#9523,#9524,#9525,#9526,#9527));
#2221=EDGE_LOOP('',(#9528,#9529,#9530,#9531));
#2222=EDGE_LOOP('',(#9532,#9533,#9534,#9535));
#2223=EDGE_LOOP('',(#9536,#9537,#9538,#9539));
#2224=EDGE_LOOP('',(#9540,#9541,#9542,#9543));
#2225=EDGE_LOOP('',(#9544,#9545,#9546,#9547));
#2226=EDGE_LOOP('',(#9548,#9549,#9550,#9551));
#2227=EDGE_LOOP('',(#9552,#9553,#9554,#9555));
#2228=EDGE_LOOP('',(#9556,#9557,#9558,#9559,#9560,#9561,#9562,#9563,#9564,
#9565,#9566,#9567,#9568,#9569));
#2229=EDGE_LOOP('',(#9570,#9571,#9572,#9573));
#2230=EDGE_LOOP('',(#9574,#9575,#9576,#9577));
#2231=EDGE_LOOP('',(#9578,#9579,#9580,#9581));
#2232=EDGE_LOOP('',(#9582,#9583,#9584,#9585));
#2233=EDGE_LOOP('',(#9586,#9587,#9588,#9589));
#2234=EDGE_LOOP('',(#9590,#9591,#9592,#9593));
#2235=EDGE_LOOP('',(#9594,#9595,#9596,#9597));
#2236=EDGE_LOOP('',(#9598,#9599,#9600,#9601));
#2237=EDGE_LOOP('',(#9602,#9603,#9604,#9605));
#2238=EDGE_LOOP('',(#9606,#9607,#9608,#9609));
#2239=EDGE_LOOP('',(#9610,#9611,#9612,#9613));
#2240=EDGE_LOOP('',(#9614,#9615,#9616,#9617,#9618,#9619,#9620,#9621));
#2241=EDGE_LOOP('',(#9622,#9623,#9624,#9625,#9626,#9627,#9628,#9629,#9630,
#9631,#9632,#9633,#9634,#9635));
#2242=EDGE_LOOP('',(#9636,#9637,#9638,#9639,#9640,#9641,#9642,#9643));
#2243=EDGE_LOOP('',(#9644,#9645,#9646,#9647));
#2244=EDGE_LOOP('',(#9648,#9649,#9650,#9651));
#2245=EDGE_LOOP('',(#9652,#9653,#9654,#9655));
#2246=EDGE_LOOP('',(#9656,#9657,#9658,#9659));
#2247=EDGE_LOOP('',(#9660,#9661,#9662,#9663));
#2248=EDGE_LOOP('',(#9664,#9665,#9666,#9667));
#2249=EDGE_LOOP('',(#9668,#9669,#9670,#9671));
#2250=EDGE_LOOP('',(#9672,#9673,#9674,#9675,#9676,#9677,#9678,#9679,#9680,
#9681,#9682,#9683,#9684,#9685));
#2251=EDGE_LOOP('',(#9686,#9687,#9688,#9689));
#2252=EDGE_LOOP('',(#9690,#9691,#9692,#9693));
#2253=EDGE_LOOP('',(#9694,#9695,#9696,#9697));
#2254=EDGE_LOOP('',(#9698,#9699,#9700,#9701));
#2255=EDGE_LOOP('',(#9702,#9703,#9704,#9705));
#2256=EDGE_LOOP('',(#9706,#9707,#9708,#9709));
#2257=EDGE_LOOP('',(#9710,#9711,#9712,#9713));
#2258=EDGE_LOOP('',(#9714,#9715,#9716,#9717));
#2259=EDGE_LOOP('',(#9718,#9719,#9720,#9721));
#2260=EDGE_LOOP('',(#9722,#9723,#9724,#9725));
#2261=EDGE_LOOP('',(#9726,#9727,#9728,#9729));
#2262=EDGE_LOOP('',(#9730,#9731,#9732,#9733,#9734,#9735,#9736,#9737));
#2263=EDGE_LOOP('',(#9738,#9739,#9740,#9741,#9742,#9743,#9744,#9745,#9746,
#9747,#9748,#9749,#9750,#9751));
#2264=EDGE_LOOP('',(#9752,#9753,#9754,#9755,#9756,#9757,#9758,#9759));
#2265=EDGE_LOOP('',(#9760,#9761,#9762,#9763));
#2266=EDGE_LOOP('',(#9764,#9765,#9766,#9767));
#2267=EDGE_LOOP('',(#9768,#9769,#9770,#9771));
#2268=EDGE_LOOP('',(#9772,#9773,#9774,#9775));
#2269=EDGE_LOOP('',(#9776,#9777,#9778,#9779));
#2270=EDGE_LOOP('',(#9780,#9781,#9782,#9783));
#2271=EDGE_LOOP('',(#9784,#9785,#9786,#9787));
#2272=EDGE_LOOP('',(#9788,#9789,#9790,#9791,#9792,#9793,#9794,#9795,#9796,
#9797,#9798,#9799,#9800,#9801));
#2273=EDGE_LOOP('',(#9802,#9803,#9804,#9805));
#2274=EDGE_LOOP('',(#9806,#9807,#9808,#9809));
#2275=EDGE_LOOP('',(#9810,#9811,#9812,#9813));
#2276=EDGE_LOOP('',(#9814,#9815,#9816,#9817));
#2277=EDGE_LOOP('',(#9818,#9819,#9820,#9821));
#2278=EDGE_LOOP('',(#9822,#9823,#9824,#9825));
#2279=EDGE_LOOP('',(#9826,#9827,#9828,#9829));
#2280=EDGE_LOOP('',(#9830,#9831,#9832,#9833));
#2281=EDGE_LOOP('',(#9834,#9835,#9836,#9837));
#2282=EDGE_LOOP('',(#9838,#9839,#9840,#9841));
#2283=EDGE_LOOP('',(#9842,#9843,#9844,#9845));
#2284=EDGE_LOOP('',(#9846,#9847,#9848,#9849,#9850,#9851,#9852,#9853));
#2285=EDGE_LOOP('',(#9854,#9855,#9856,#9857,#9858,#9859,#9860,#9861,#9862,
#9863,#9864,#9865,#9866,#9867));
#2286=EDGE_LOOP('',(#9868,#9869,#9870,#9871,#9872,#9873,#9874,#9875));
#2287=EDGE_LOOP('',(#9876,#9877,#9878,#9879));
#2288=EDGE_LOOP('',(#9880,#9881,#9882,#9883));
#2289=EDGE_LOOP('',(#9884,#9885,#9886,#9887));
#2290=EDGE_LOOP('',(#9888,#9889,#9890,#9891));
#2291=EDGE_LOOP('',(#9892,#9893,#9894,#9895));
#2292=EDGE_LOOP('',(#9896,#9897,#9898,#9899));
#2293=EDGE_LOOP('',(#9900,#9901,#9902,#9903));
#2294=EDGE_LOOP('',(#9904,#9905,#9906,#9907,#9908,#9909,#9910,#9911,#9912,
#9913,#9914,#9915,#9916,#9917));
#2295=EDGE_LOOP('',(#9918,#9919,#9920,#9921));
#2296=EDGE_LOOP('',(#9922,#9923,#9924,#9925));
#2297=EDGE_LOOP('',(#9926,#9927,#9928,#9929));
#2298=EDGE_LOOP('',(#9930,#9931,#9932,#9933));
#2299=EDGE_LOOP('',(#9934,#9935,#9936,#9937));
#2300=EDGE_LOOP('',(#9938,#9939,#9940,#9941));
#2301=EDGE_LOOP('',(#9942,#9943,#9944,#9945));
#2302=EDGE_LOOP('',(#9946,#9947,#9948,#9949));
#2303=EDGE_LOOP('',(#9950,#9951,#9952,#9953));
#2304=EDGE_LOOP('',(#9954,#9955,#9956,#9957));
#2305=EDGE_LOOP('',(#9958,#9959,#9960,#9961));
#2306=EDGE_LOOP('',(#9962,#9963,#9964,#9965,#9966,#9967,#9968,#9969));
#2307=EDGE_LOOP('',(#9970,#9971,#9972,#9973,#9974,#9975,#9976,#9977,#9978,
#9979,#9980,#9981,#9982,#9983));
#2308=EDGE_LOOP('',(#9984,#9985,#9986,#9987,#9988,#9989,#9990,#9991));
#2309=EDGE_LOOP('',(#9992,#9993,#9994,#9995));
#2310=EDGE_LOOP('',(#9996,#9997,#9998,#9999));
#2311=EDGE_LOOP('',(#10000,#10001,#10002,#10003));
#2312=EDGE_LOOP('',(#10004,#10005,#10006,#10007));
#2313=EDGE_LOOP('',(#10008,#10009,#10010,#10011));
#2314=EDGE_LOOP('',(#10012,#10013,#10014,#10015));
#2315=EDGE_LOOP('',(#10016,#10017,#10018,#10019));
#2316=EDGE_LOOP('',(#10020,#10021,#10022,#10023,#10024,#10025,#10026,#10027,
#10028,#10029,#10030,#10031,#10032,#10033));
#2317=EDGE_LOOP('',(#10034,#10035,#10036,#10037));
#2318=EDGE_LOOP('',(#10038,#10039,#10040,#10041));
#2319=EDGE_LOOP('',(#10042,#10043,#10044,#10045));
#2320=EDGE_LOOP('',(#10046,#10047,#10048,#10049));
#2321=EDGE_LOOP('',(#10050,#10051,#10052,#10053));
#2322=EDGE_LOOP('',(#10054,#10055,#10056,#10057));
#2323=EDGE_LOOP('',(#10058,#10059,#10060,#10061));
#2324=EDGE_LOOP('',(#10062,#10063,#10064,#10065));
#2325=EDGE_LOOP('',(#10066,#10067,#10068,#10069));
#2326=EDGE_LOOP('',(#10070,#10071,#10072,#10073));
#2327=EDGE_LOOP('',(#10074,#10075,#10076,#10077));
#2328=EDGE_LOOP('',(#10078,#10079,#10080,#10081,#10082,#10083,#10084,#10085));
#2329=EDGE_LOOP('',(#10086,#10087,#10088,#10089,#10090,#10091,#10092,#10093,
#10094,#10095,#10096,#10097,#10098,#10099));
#2330=EDGE_LOOP('',(#10100,#10101,#10102,#10103));
#2331=EDGE_LOOP('',(#10104,#10105,#10106,#10107));
#2332=EDGE_LOOP('',(#10108,#10109,#10110,#10111));
#2333=EDGE_LOOP('',(#10112,#10113,#10114,#10115));
#2334=EDGE_LOOP('',(#10116,#10117,#10118,#10119));
#2335=EDGE_LOOP('',(#10120,#10121,#10122,#10123));
#2336=EDGE_LOOP('',(#10124,#10125,#10126,#10127));
#2337=EDGE_LOOP('',(#10128,#10129,#10130,#10131));
#2338=EDGE_LOOP('',(#10132,#10133,#10134,#10135));
#2339=EDGE_LOOP('',(#10136,#10137,#10138,#10139));
#2340=EDGE_LOOP('',(#10140,#10141,#10142,#10143));
#2341=EDGE_LOOP('',(#10144,#10145,#10146,#10147));
#2342=EDGE_LOOP('',(#10148,#10149,#10150,#10151));
#2343=EDGE_LOOP('',(#10152,#10153,#10154,#10155));
#2344=EDGE_LOOP('',(#10156,#10157,#10158,#10159));
#2345=EDGE_LOOP('',(#10160,#10161,#10162,#10163));
#2346=EDGE_LOOP('',(#10164,#10165,#10166,#10167));
#2347=EDGE_LOOP('',(#10168,#10169,#10170,#10171));
#2348=EDGE_LOOP('',(#10172,#10173,#10174,#10175));
#2349=EDGE_LOOP('',(#10176,#10177,#10178,#10179));
#2350=EDGE_LOOP('',(#10180,#10181,#10182,#10183,#10184,#10185));
#2351=EDGE_LOOP('',(#10186));
#2352=EDGE_LOOP('',(#10187,#10188,#10189,#10190,#10191,#10192));
#2353=EDGE_LOOP('',(#10193,#10194,#10195,#10196));
#2354=EDGE_LOOP('',(#10197,#10198,#10199,#10200));
#2355=EDGE_LOOP('',(#10201,#10202,#10203,#10204));
#2356=EDGE_LOOP('',(#10205));
#2357=EDGE_LOOP('',(#10206));
#2358=EDGE_LOOP('',(#10207,#10208,#10209,#10210));
#2359=EDGE_LOOP('',(#10211,#10212,#10213,#10214));
#2360=EDGE_LOOP('',(#10215,#10216,#10217,#10218));
#2361=EDGE_LOOP('',(#10219));
#2362=EDGE_LOOP('',(#10220));
#2363=EDGE_LOOP('',(#10221,#10222,#10223,#10224));
#2364=EDGE_LOOP('',(#10225,#10226,#10227,#10228));
#2365=EDGE_LOOP('',(#10229,#10230,#10231,#10232));
#2366=EDGE_LOOP('',(#10233));
#2367=EDGE_LOOP('',(#10234,#10235,#10236,#10237));
#2368=EDGE_LOOP('',(#10238,#10239,#10240,#10241));
#2369=EDGE_LOOP('',(#10242,#10243,#10244,#10245));
#2370=EDGE_LOOP('',(#10246,#10247,#10248,#10249));
#2371=EDGE_LOOP('',(#10250,#10251,#10252,#10253));
#2372=EDGE_LOOP('',(#10254,#10255,#10256,#10257));
#2373=EDGE_LOOP('',(#10258,#10259,#10260,#10261,#10262,#10263));
#2374=EDGE_LOOP('',(#10264,#10265,#10266,#10267,#10268,#10269));
#2375=LINE('',#15434,#3528);
#2376=LINE('',#15440,#3529);
#2377=LINE('',#15446,#3530);
#2378=LINE('',#15452,#3531);
#2379=LINE('',#15458,#3532);
#2380=LINE('',#15464,#3533);
#2381=LINE('',#15469,#3534);
#2382=LINE('',#15471,#3535);
#2383=LINE('',#15473,#3536);
#2384=LINE('',#15474,#3537);
#2385=LINE('',#15477,#3538);
#2386=LINE('',#15479,#3539);
#2387=LINE('',#15480,#3540);
#2388=LINE('',#15483,#3541);
#2389=LINE('',#15485,#3542);
#2390=LINE('',#15486,#3543);
#2391=LINE('',#15488,#3544);
#2392=LINE('',#15489,#3545);
#2393=LINE('',#15496,#3546);
#2394=LINE('',#15498,#3547);
#2395=LINE('',#15500,#3548);
#2396=LINE('',#15501,#3549);
#2397=LINE('',#15504,#3550);
#2398=LINE('',#15506,#3551);
#2399=LINE('',#15507,#3552);
#2400=LINE('',#15510,#3553);
#2401=LINE('',#15512,#3554);
#2402=LINE('',#15513,#3555);
#2403=LINE('',#15515,#3556);
#2404=LINE('',#15516,#3557);
#2405=LINE('',#15523,#3558);
#2406=LINE('',#15525,#3559);
#2407=LINE('',#15527,#3560);
#2408=LINE('',#15528,#3561);
#2409=LINE('',#15531,#3562);
#2410=LINE('',#15533,#3563);
#2411=LINE('',#15534,#3564);
#2412=LINE('',#15537,#3565);
#2413=LINE('',#15539,#3566);
#2414=LINE('',#15540,#3567);
#2415=LINE('',#15542,#3568);
#2416=LINE('',#15543,#3569);
#2417=LINE('',#15551,#3570);
#2418=LINE('',#15557,#3571);
#2419=LINE('',#15566,#3572);
#2420=LINE('',#15572,#3573);
#2421=LINE('',#15581,#3574);
#2422=LINE('',#15587,#3575);
#2423=LINE('',#15596,#3576);
#2424=LINE('',#15602,#3577);
#2425=LINE('',#15611,#3578);
#2426=LINE('',#15617,#3579);
#2427=LINE('',#15623,#3580);
#2428=LINE('',#15629,#3581);
#2429=LINE('',#15635,#3582);
#2430=LINE('',#15641,#3583);
#2431=LINE('',#15647,#3584);
#2432=LINE('',#15652,#3585);
#2433=LINE('',#15654,#3586);
#2434=LINE('',#15656,#3587);
#2435=LINE('',#15657,#3588);
#2436=LINE('',#15660,#3589);
#2437=LINE('',#15662,#3590);
#2438=LINE('',#15663,#3591);
#2439=LINE('',#15667,#3592);
#2440=LINE('',#15669,#3593);
#2441=LINE('',#15671,#3594);
#2442=LINE('',#15672,#3595);
#2443=LINE('',#15675,#3596);
#2444=LINE('',#15676,#3597);
#2445=LINE('',#15677,#3598);
#2446=LINE('',#15680,#3599);
#2447=LINE('',#15681,#3600);
#2448=LINE('',#15682,#3601);
#2449=LINE('',#15684,#3602);
#2450=LINE('',#15692,#3603);
#2451=LINE('',#15699,#3604);
#2452=LINE('',#15706,#3605);
#2453=LINE('',#15713,#3606);
#2454=LINE('',#15720,#3607);
#2455=LINE('',#15728,#3608);
#2456=LINE('',#15732,#3609);
#2457=LINE('',#15734,#3610);
#2458=LINE('',#15736,#3611);
#2459=LINE('',#15737,#3612);
#2460=LINE('',#15740,#3613);
#2461=LINE('',#15742,#3614);
#2462=LINE('',#15743,#3615);
#2463=LINE('',#15746,#3616);
#2464=LINE('',#15748,#3617);
#2465=LINE('',#15749,#3618);
#2466=LINE('',#15751,#3619);
#2467=LINE('',#15752,#3620);
#2468=LINE('',#15759,#3621);
#2469=LINE('',#15761,#3622);
#2470=LINE('',#15763,#3623);
#2471=LINE('',#15764,#3624);
#2472=LINE('',#15767,#3625);
#2473=LINE('',#15769,#3626);
#2474=LINE('',#15770,#3627);
#2475=LINE('',#15773,#3628);
#2476=LINE('',#15775,#3629);
#2477=LINE('',#15776,#3630);
#2478=LINE('',#15779,#3631);
#2479=LINE('',#15781,#3632);
#2480=LINE('',#15782,#3633);
#2481=LINE('',#15785,#3634);
#2482=LINE('',#15787,#3635);
#2483=LINE('',#15788,#3636);
#2484=LINE('',#15790,#3637);
#2485=LINE('',#15791,#3638);
#2486=LINE('',#15801,#3639);
#2487=LINE('',#15805,#3640);
#2488=LINE('',#15812,#3641);
#2489=LINE('',#15814,#3642);
#2490=LINE('',#15816,#3643);
#2491=LINE('',#15817,#3644);
#2492=LINE('',#15820,#3645);
#2493=LINE('',#15822,#3646);
#2494=LINE('',#15823,#3647);
#2495=LINE('',#15826,#3648);
#2496=LINE('',#15828,#3649);
#2497=LINE('',#15829,#3650);
#2498=LINE('',#15832,#3651);
#2499=LINE('',#15834,#3652);
#2500=LINE('',#15835,#3653);
#2501=LINE('',#15838,#3654);
#2502=LINE('',#15840,#3655);
#2503=LINE('',#15841,#3656);
#2504=LINE('',#15843,#3657);
#2505=LINE('',#15844,#3658);
#2506=LINE('',#15854,#3659);
#2507=LINE('',#15858,#3660);
#2508=LINE('',#15865,#3661);
#2509=LINE('',#15867,#3662);
#2510=LINE('',#15869,#3663);
#2511=LINE('',#15870,#3664);
#2512=LINE('',#15873,#3665);
#2513=LINE('',#15875,#3666);
#2514=LINE('',#15876,#3667);
#2515=LINE('',#15879,#3668);
#2516=LINE('',#15881,#3669);
#2517=LINE('',#15882,#3670);
#2518=LINE('',#15885,#3671);
#2519=LINE('',#15887,#3672);
#2520=LINE('',#15888,#3673);
#2521=LINE('',#15891,#3674);
#2522=LINE('',#15893,#3675);
#2523=LINE('',#15894,#3676);
#2524=LINE('',#15896,#3677);
#2525=LINE('',#15897,#3678);
#2526=LINE('',#15907,#3679);
#2527=LINE('',#15911,#3680);
#2528=LINE('',#15918,#3681);
#2529=LINE('',#15920,#3682);
#2530=LINE('',#15922,#3683);
#2531=LINE('',#15923,#3684);
#2532=LINE('',#15926,#3685);
#2533=LINE('',#15928,#3686);
#2534=LINE('',#15929,#3687);
#2535=LINE('',#15932,#3688);
#2536=LINE('',#15934,#3689);
#2537=LINE('',#15935,#3690);
#2538=LINE('',#15938,#3691);
#2539=LINE('',#15940,#3692);
#2540=LINE('',#15941,#3693);
#2541=LINE('',#15944,#3694);
#2542=LINE('',#15946,#3695);
#2543=LINE('',#15947,#3696);
#2544=LINE('',#15949,#3697);
#2545=LINE('',#15950,#3698);
#2546=LINE('',#15960,#3699);
#2547=LINE('',#15964,#3700);
#2548=LINE('',#15972,#3701);
#2549=LINE('',#15977,#3702);
#2550=LINE('',#15981,#3703);
#2551=LINE('',#15985,#3704);
#2552=LINE('',#15992,#3705);
#2553=LINE('',#15995,#3706);
#2554=LINE('',#15997,#3707);
#2555=LINE('',#16000,#3708);
#2556=LINE('',#16003,#3709);
#2557=LINE('',#16006,#3710);
#2558=LINE('',#16014,#3711);
#2559=LINE('',#16016,#3712);
#2560=LINE('',#16021,#3713);
#2561=LINE('',#16024,#3714);
#2562=LINE('',#16028,#3715);
#2563=LINE('',#16031,#3716);
#2564=LINE('',#16033,#3717);
#2565=LINE('',#16034,#3718);
#2566=LINE('',#16038,#3719);
#2567=LINE('',#16040,#3720);
#2568=LINE('',#16043,#3721);
#2569=LINE('',#16044,#3722);
#2570=LINE('',#16048,#3723);
#2571=LINE('',#16050,#3724);
#2572=LINE('',#16052,#3725);
#2573=LINE('',#16053,#3726);
#2574=LINE('',#16054,#3727);
#2575=LINE('',#16056,#3728);
#2576=LINE('',#16057,#3729);
#2577=LINE('',#16059,#3730);
#2578=LINE('',#16060,#3731);
#2579=LINE('',#16061,#3732);
#2580=LINE('',#16071,#3733);
#2581=LINE('',#16074,#3734);
#2582=LINE('',#16080,#3735);
#2583=LINE('',#16082,#3736);
#2584=LINE('',#16084,#3737);
#2585=LINE('',#16086,#3738);
#2586=LINE('',#16087,#3739);
#2587=LINE('',#16090,#3740);
#2588=LINE('',#16091,#3741);
#2589=LINE('',#16094,#3742);
#2590=LINE('',#16096,#3743);
#2591=LINE('',#16097,#3744);
#2592=LINE('',#16099,#3745);
#2593=LINE('',#16101,#3746);
#2594=LINE('',#16102,#3747);
#2595=LINE('',#16104,#3748);
#2596=LINE('',#16109,#3749);
#2597=LINE('',#16113,#3750);
#2598=LINE('',#16117,#3751);
#2599=LINE('',#16118,#3752);
#2600=LINE('',#16119,#3753);
#2601=LINE('',#16122,#3754);
#2602=LINE('',#16123,#3755);
#2603=LINE('',#16126,#3756);
#2604=LINE('',#16127,#3757);
#2605=LINE('',#16129,#3758);
#2606=LINE('',#16136,#3759);
#2607=LINE('',#16191,#3760);
#2608=LINE('',#16263,#3761);
#2609=LINE('',#16308,#3762);
#2610=LINE('',#16476,#3763);
#2611=LINE('',#16547,#3764);
#2612=LINE('',#16550,#3765);
#2613=LINE('',#16621,#3766);
#2614=LINE('',#16631,#3767);
#2615=LINE('',#16636,#3768);
#2616=LINE('',#16644,#3769);
#2617=LINE('',#16650,#3770);
#2618=LINE('',#16658,#3771);
#2619=LINE('',#16660,#3772);
#2620=LINE('',#16662,#3773);
#2621=LINE('',#16663,#3774);
#2622=LINE('',#16666,#3775);
#2623=LINE('',#16668,#3776);
#2624=LINE('',#16669,#3777);
#2625=LINE('',#16672,#3778);
#2626=LINE('',#16674,#3779);
#2627=LINE('',#16675,#3780);
#2628=LINE('',#16678,#3781);
#2629=LINE('',#16680,#3782);
#2630=LINE('',#16681,#3783);
#2631=LINE('',#16684,#3784);
#2632=LINE('',#16686,#3785);
#2633=LINE('',#16687,#3786);
#2634=LINE('',#16689,#3787);
#2635=LINE('',#16690,#3788);
#2636=LINE('',#16702,#3789);
#2637=LINE('',#16706,#3790);
#2638=LINE('',#16710,#3791);
#2639=LINE('',#16717,#3792);
#2640=LINE('',#16719,#3793);
#2641=LINE('',#16724,#3794);
#2642=LINE('',#16726,#3795);
#2643=LINE('',#16728,#3796);
#2644=LINE('',#16729,#3797);
#2645=LINE('',#16732,#3798);
#2646=LINE('',#16734,#3799);
#2647=LINE('',#16735,#3800);
#2648=LINE('',#16738,#3801);
#2649=LINE('',#16740,#3802);
#2650=LINE('',#16741,#3803);
#2651=LINE('',#16744,#3804);
#2652=LINE('',#16746,#3805);
#2653=LINE('',#16747,#3806);
#2654=LINE('',#16750,#3807);
#2655=LINE('',#16752,#3808);
#2656=LINE('',#16753,#3809);
#2657=LINE('',#16755,#3810);
#2658=LINE('',#16756,#3811);
#2659=LINE('',#16768,#3812);
#2660=LINE('',#16772,#3813);
#2661=LINE('',#16776,#3814);
#2662=LINE('',#16783,#3815);
#2663=LINE('',#16785,#3816);
#2664=LINE('',#16816,#3817);
#2665=LINE('',#16818,#3818);
#2666=LINE('',#16820,#3819);
#2667=LINE('',#16821,#3820);
#2668=LINE('',#16826,#3821);
#2669=LINE('',#16827,#3822);
#2670=LINE('',#16830,#3823);
#2671=LINE('',#16832,#3824);
#2672=LINE('',#16833,#3825);
#2673=LINE('',#16835,#3826);
#2674=LINE('',#16842,#3827);
#2675=LINE('',#16849,#3828);
#2676=LINE('',#16858,#3829);
#2677=LINE('',#16866,#3830);
#2678=LINE('',#16883,#3831);
#2679=LINE('',#16934,#3832);
#2680=LINE('',#16939,#3833);
#2681=LINE('',#16945,#3834);
#2682=LINE('',#16953,#3835);
#2683=LINE('',#16970,#3836);
#2684=LINE('',#17021,#3837);
#2685=LINE('',#17025,#3838);
#2686=LINE('',#17027,#3839);
#2687=LINE('',#17029,#3840);
#2688=LINE('',#17030,#3841);
#2689=LINE('',#17033,#3842);
#2690=LINE('',#17035,#3843);
#2691=LINE('',#17036,#3844);
#2692=LINE('',#17039,#3845);
#2693=LINE('',#17041,#3846);
#2694=LINE('',#17042,#3847);
#2695=LINE('',#17060,#3848);
#2696=LINE('',#17063,#3849);
#2697=LINE('',#17066,#3850);
#2698=LINE('',#17072,#3851);
#2699=LINE('',#17089,#3852);
#2700=LINE('',#17140,#3853);
#2701=LINE('',#17145,#3854);
#2702=LINE('',#17151,#3855);
#2703=LINE('',#17159,#3856);
#2704=LINE('',#17176,#3857);
#2705=LINE('',#17227,#3858);
#2706=LINE('',#17232,#3859);
#2707=LINE('',#17238,#3860);
#2708=LINE('',#17247,#3861);
#2709=LINE('',#17253,#3862);
#2710=LINE('',#17261,#3863);
#2711=LINE('',#17263,#3864);
#2712=LINE('',#17265,#3865);
#2713=LINE('',#17266,#3866);
#2714=LINE('',#17269,#3867);
#2715=LINE('',#17271,#3868);
#2716=LINE('',#17272,#3869);
#2717=LINE('',#17275,#3870);
#2718=LINE('',#17277,#3871);
#2719=LINE('',#17278,#3872);
#2720=LINE('',#17281,#3873);
#2721=LINE('',#17283,#3874);
#2722=LINE('',#17284,#3875);
#2723=LINE('',#17287,#3876);
#2724=LINE('',#17289,#3877);
#2725=LINE('',#17290,#3878);
#2726=LINE('',#17292,#3879);
#2727=LINE('',#17293,#3880);
#2728=LINE('',#17301,#3881);
#2729=LINE('',#17305,#3882);
#2730=LINE('',#17309,#3883);
#2731=LINE('',#17353,#3884);
#2732=LINE('',#17392,#3885);
#2733=LINE('',#17397,#3886);
#2734=LINE('',#17399,#3887);
#2735=LINE('',#17401,#3888);
#2736=LINE('',#17402,#3889);
#2737=LINE('',#17405,#3890);
#2738=LINE('',#17407,#3891);
#2739=LINE('',#17408,#3892);
#2740=LINE('',#17411,#3893);
#2741=LINE('',#17413,#3894);
#2742=LINE('',#17414,#3895);
#2743=LINE('',#17417,#3896);
#2744=LINE('',#17419,#3897);
#2745=LINE('',#17420,#3898);
#2746=LINE('',#17423,#3899);
#2747=LINE('',#17425,#3900);
#2748=LINE('',#17426,#3901);
#2749=LINE('',#17429,#3902);
#2750=LINE('',#17431,#3903);
#2751=LINE('',#17432,#3904);
#2752=LINE('',#17435,#3905);
#2753=LINE('',#17437,#3906);
#2754=LINE('',#17438,#3907);
#2755=LINE('',#17441,#3908);
#2756=LINE('',#17443,#3909);
#2757=LINE('',#17444,#3910);
#2758=LINE('',#17447,#3911);
#2759=LINE('',#17449,#3912);
#2760=LINE('',#17450,#3913);
#2761=LINE('',#17453,#3914);
#2762=LINE('',#17455,#3915);
#2763=LINE('',#17456,#3916);
#2764=LINE('',#17459,#3917);
#2765=LINE('',#17461,#3918);
#2766=LINE('',#17462,#3919);
#2767=LINE('',#17465,#3920);
#2768=LINE('',#17467,#3921);
#2769=LINE('',#17468,#3922);
#2770=LINE('',#17471,#3923);
#2771=LINE('',#17473,#3924);
#2772=LINE('',#17474,#3925);
#2773=LINE('',#17477,#3926);
#2774=LINE('',#17479,#3927);
#2775=LINE('',#17480,#3928);
#2776=LINE('',#17483,#3929);
#2777=LINE('',#17485,#3930);
#2778=LINE('',#17486,#3931);
#2779=LINE('',#17489,#3932);
#2780=LINE('',#17491,#3933);
#2781=LINE('',#17492,#3934);
#2782=LINE('',#17495,#3935);
#2783=LINE('',#17497,#3936);
#2784=LINE('',#17498,#3937);
#2785=LINE('',#17500,#3938);
#2786=LINE('',#17501,#3939);
#2787=LINE('',#17523,#3940);
#2788=LINE('',#17525,#3941);
#2789=LINE('',#17527,#3942);
#2790=LINE('',#17529,#3943);
#2791=LINE('',#17531,#3944);
#2792=LINE('',#17533,#3945);
#2793=LINE('',#17535,#3946);
#2794=LINE('',#17537,#3947);
#2795=LINE('',#17539,#3948);
#2796=LINE('',#17541,#3949);
#2797=LINE('',#17545,#3950);
#2798=LINE('',#17547,#3951);
#2799=LINE('',#17549,#3952);
#2800=LINE('',#17551,#3953);
#2801=LINE('',#17553,#3954);
#2802=LINE('',#17555,#3955);
#2803=LINE('',#17557,#3956);
#2804=LINE('',#17559,#3957);
#2805=LINE('',#17561,#3958);
#2806=LINE('',#17563,#3959);
#2807=LINE('',#17570,#3960);
#2808=LINE('',#17571,#3961);
#2809=LINE('',#17573,#3962);
#2810=LINE('',#17574,#3963);
#2811=LINE('',#17577,#3964);
#2812=LINE('',#17579,#3965);
#2813=LINE('',#17580,#3966);
#2814=LINE('',#17583,#3967);
#2815=LINE('',#17585,#3968);
#2816=LINE('',#17586,#3969);
#2817=LINE('',#17589,#3970);
#2818=LINE('',#17591,#3971);
#2819=LINE('',#17592,#3972);
#2820=LINE('',#17595,#3973);
#2821=LINE('',#17597,#3974);
#2822=LINE('',#17598,#3975);
#2823=LINE('',#17601,#3976);
#2824=LINE('',#17603,#3977);
#2825=LINE('',#17604,#3978);
#2826=LINE('',#17607,#3979);
#2827=LINE('',#17609,#3980);
#2828=LINE('',#17610,#3981);
#2829=LINE('',#17613,#3982);
#2830=LINE('',#17614,#3983);
#2831=LINE('',#17615,#3984);
#2832=LINE('',#17618,#3985);
#2833=LINE('',#17619,#3986);
#2834=LINE('',#17622,#3987);
#2835=LINE('',#17623,#3988);
#2836=LINE('',#17626,#3989);
#2837=LINE('',#17627,#3990);
#2838=LINE('',#17630,#3991);
#2839=LINE('',#17631,#3992);
#2840=LINE('',#17634,#3993);
#2841=LINE('',#17635,#3994);
#2842=LINE('',#17638,#3995);
#2843=LINE('',#17639,#3996);
#2844=LINE('',#17642,#3997);
#2845=LINE('',#17643,#3998);
#2846=LINE('',#17646,#3999);
#2847=LINE('',#17647,#4000);
#2848=LINE('',#17650,#4001);
#2849=LINE('',#17651,#4002);
#2850=LINE('',#17653,#4003);
#2851=LINE('',#17674,#4004);
#2852=LINE('',#17675,#4005);
#2853=LINE('',#17677,#4006);
#2854=LINE('',#17678,#4007);
#2855=LINE('',#17681,#4008);
#2856=LINE('',#17683,#4009);
#2857=LINE('',#17684,#4010);
#2858=LINE('',#17687,#4011);
#2859=LINE('',#17689,#4012);
#2860=LINE('',#17690,#4013);
#2861=LINE('',#17693,#4014);
#2862=LINE('',#17695,#4015);
#2863=LINE('',#17696,#4016);
#2864=LINE('',#17699,#4017);
#2865=LINE('',#17701,#4018);
#2866=LINE('',#17702,#4019);
#2867=LINE('',#17705,#4020);
#2868=LINE('',#17707,#4021);
#2869=LINE('',#17708,#4022);
#2870=LINE('',#17711,#4023);
#2871=LINE('',#17713,#4024);
#2872=LINE('',#17714,#4025);
#2873=LINE('',#17717,#4026);
#2874=LINE('',#17718,#4027);
#2875=LINE('',#17719,#4028);
#2876=LINE('',#17722,#4029);
#2877=LINE('',#17723,#4030);
#2878=LINE('',#17726,#4031);
#2879=LINE('',#17727,#4032);
#2880=LINE('',#17730,#4033);
#2881=LINE('',#17731,#4034);
#2882=LINE('',#17734,#4035);
#2883=LINE('',#17735,#4036);
#2884=LINE('',#17738,#4037);
#2885=LINE('',#17739,#4038);
#2886=LINE('',#17742,#4039);
#2887=LINE('',#17743,#4040);
#2888=LINE('',#17746,#4041);
#2889=LINE('',#17747,#4042);
#2890=LINE('',#17750,#4043);
#2891=LINE('',#17751,#4044);
#2892=LINE('',#17754,#4045);
#2893=LINE('',#17755,#4046);
#2894=LINE('',#17757,#4047);
#2895=LINE('',#17778,#4048);
#2896=LINE('',#17821,#4049);
#2897=LINE('',#17863,#4050);
#2898=LINE('',#17868,#4051);
#2899=LINE('',#17870,#4052);
#2900=LINE('',#17872,#4053);
#2901=LINE('',#17873,#4054);
#2902=LINE('',#17876,#4055);
#2903=LINE('',#17878,#4056);
#2904=LINE('',#17879,#4057);
#2905=LINE('',#17882,#4058);
#2906=LINE('',#17884,#4059);
#2907=LINE('',#17885,#4060);
#2908=LINE('',#17888,#4061);
#2909=LINE('',#17890,#4062);
#2910=LINE('',#17891,#4063);
#2911=LINE('',#17894,#4064);
#2912=LINE('',#17896,#4065);
#2913=LINE('',#17897,#4066);
#2914=LINE('',#17900,#4067);
#2915=LINE('',#17902,#4068);
#2916=LINE('',#17903,#4069);
#2917=LINE('',#17906,#4070);
#2918=LINE('',#17908,#4071);
#2919=LINE('',#17909,#4072);
#2920=LINE('',#17912,#4073);
#2921=LINE('',#17914,#4074);
#2922=LINE('',#17915,#4075);
#2923=LINE('',#17918,#4076);
#2924=LINE('',#17920,#4077);
#2925=LINE('',#17921,#4078);
#2926=LINE('',#17924,#4079);
#2927=LINE('',#17926,#4080);
#2928=LINE('',#17927,#4081);
#2929=LINE('',#17930,#4082);
#2930=LINE('',#17932,#4083);
#2931=LINE('',#17933,#4084);
#2932=LINE('',#17936,#4085);
#2933=LINE('',#17938,#4086);
#2934=LINE('',#17939,#4087);
#2935=LINE('',#17942,#4088);
#2936=LINE('',#17944,#4089);
#2937=LINE('',#17945,#4090);
#2938=LINE('',#17948,#4091);
#2939=LINE('',#17950,#4092);
#2940=LINE('',#17951,#4093);
#2941=LINE('',#17954,#4094);
#2942=LINE('',#17956,#4095);
#2943=LINE('',#17957,#4096);
#2944=LINE('',#17960,#4097);
#2945=LINE('',#17962,#4098);
#2946=LINE('',#17963,#4099);
#2947=LINE('',#17966,#4100);
#2948=LINE('',#17968,#4101);
#2949=LINE('',#17969,#4102);
#2950=LINE('',#17971,#4103);
#2951=LINE('',#17972,#4104);
#2952=LINE('',#17992,#4105);
#2953=LINE('',#17994,#4106);
#2954=LINE('',#17996,#4107);
#2955=LINE('',#17998,#4108);
#2956=LINE('',#18000,#4109);
#2957=LINE('',#18002,#4110);
#2958=LINE('',#18004,#4111);
#2959=LINE('',#18006,#4112);
#2960=LINE('',#18008,#4113);
#2961=LINE('',#18010,#4114);
#2962=LINE('',#18014,#4115);
#2963=LINE('',#18016,#4116);
#2964=LINE('',#18018,#4117);
#2965=LINE('',#18020,#4118);
#2966=LINE('',#18022,#4119);
#2967=LINE('',#18024,#4120);
#2968=LINE('',#18026,#4121);
#2969=LINE('',#18028,#4122);
#2970=LINE('',#18030,#4123);
#2971=LINE('',#18032,#4124);
#2972=LINE('',#18041,#4125);
#2973=LINE('',#18042,#4126);
#2974=LINE('',#18043,#4127);
#2975=LINE('',#18046,#4128);
#2976=LINE('',#18047,#4129);
#2977=LINE('',#18050,#4130);
#2978=LINE('',#18051,#4131);
#2979=LINE('',#18054,#4132);
#2980=LINE('',#18055,#4133);
#2981=LINE('',#18058,#4134);
#2982=LINE('',#18059,#4135);
#2983=LINE('',#18062,#4136);
#2984=LINE('',#18063,#4137);
#2985=LINE('',#18066,#4138);
#2986=LINE('',#18067,#4139);
#2987=LINE('',#18070,#4140);
#2988=LINE('',#18071,#4141);
#2989=LINE('',#18074,#4142);
#2990=LINE('',#18075,#4143);
#2991=LINE('',#18078,#4144);
#2992=LINE('',#18080,#4145);
#2993=LINE('',#18081,#4146);
#2994=LINE('',#18084,#4147);
#2995=LINE('',#18086,#4148);
#2996=LINE('',#18087,#4149);
#2997=LINE('',#18090,#4150);
#2998=LINE('',#18092,#4151);
#2999=LINE('',#18093,#4152);
#3000=LINE('',#18096,#4153);
#3001=LINE('',#18098,#4154);
#3002=LINE('',#18099,#4155);
#3003=LINE('',#18102,#4156);
#3004=LINE('',#18104,#4157);
#3005=LINE('',#18105,#4158);
#3006=LINE('',#18108,#4159);
#3007=LINE('',#18110,#4160);
#3008=LINE('',#18111,#4161);
#3009=LINE('',#18114,#4162);
#3010=LINE('',#18116,#4163);
#3011=LINE('',#18117,#4164);
#3012=LINE('',#18120,#4165);
#3013=LINE('',#18121,#4166);
#3014=LINE('',#18122,#4167);
#3015=LINE('',#18124,#4168);
#3016=LINE('',#18145,#4169);
#3017=LINE('',#18146,#4170);
#3018=LINE('',#18147,#4171);
#3019=LINE('',#18150,#4172);
#3020=LINE('',#18151,#4173);
#3021=LINE('',#18154,#4174);
#3022=LINE('',#18155,#4175);
#3023=LINE('',#18158,#4176);
#3024=LINE('',#18159,#4177);
#3025=LINE('',#18162,#4178);
#3026=LINE('',#18163,#4179);
#3027=LINE('',#18166,#4180);
#3028=LINE('',#18167,#4181);
#3029=LINE('',#18170,#4182);
#3030=LINE('',#18171,#4183);
#3031=LINE('',#18174,#4184);
#3032=LINE('',#18175,#4185);
#3033=LINE('',#18178,#4186);
#3034=LINE('',#18179,#4187);
#3035=LINE('',#18182,#4188);
#3036=LINE('',#18184,#4189);
#3037=LINE('',#18185,#4190);
#3038=LINE('',#18188,#4191);
#3039=LINE('',#18190,#4192);
#3040=LINE('',#18191,#4193);
#3041=LINE('',#18194,#4194);
#3042=LINE('',#18196,#4195);
#3043=LINE('',#18197,#4196);
#3044=LINE('',#18200,#4197);
#3045=LINE('',#18202,#4198);
#3046=LINE('',#18203,#4199);
#3047=LINE('',#18206,#4200);
#3048=LINE('',#18208,#4201);
#3049=LINE('',#18209,#4202);
#3050=LINE('',#18212,#4203);
#3051=LINE('',#18214,#4204);
#3052=LINE('',#18215,#4205);
#3053=LINE('',#18218,#4206);
#3054=LINE('',#18220,#4207);
#3055=LINE('',#18221,#4208);
#3056=LINE('',#18224,#4209);
#3057=LINE('',#18225,#4210);
#3058=LINE('',#18226,#4211);
#3059=LINE('',#18228,#4212);
#3060=LINE('',#18249,#4213);
#3061=LINE('',#18255,#4214);
#3062=LINE('',#18257,#4215);
#3063=LINE('',#18259,#4216);
#3064=LINE('',#18261,#4217);
#3065=LINE('',#18263,#4218);
#3066=LINE('',#18265,#4219);
#3067=LINE('',#18267,#4220);
#3068=LINE('',#18269,#4221);
#3069=LINE('',#18273,#4222);
#3070=LINE('',#18275,#4223);
#3071=LINE('',#18277,#4224);
#3072=LINE('',#18279,#4225);
#3073=LINE('',#18281,#4226);
#3074=LINE('',#18283,#4227);
#3075=LINE('',#18285,#4228);
#3076=LINE('',#18287,#4229);
#3077=LINE('',#18291,#4230);
#3078=LINE('',#18293,#4231);
#3079=LINE('',#18295,#4232);
#3080=LINE('',#18297,#4233);
#3081=LINE('',#18299,#4234);
#3082=LINE('',#18301,#4235);
#3083=LINE('',#18303,#4236);
#3084=LINE('',#18305,#4237);
#3085=LINE('',#18309,#4238);
#3086=LINE('',#18311,#4239);
#3087=LINE('',#18313,#4240);
#3088=LINE('',#18315,#4241);
#3089=LINE('',#18317,#4242);
#3090=LINE('',#18319,#4243);
#3091=LINE('',#18321,#4244);
#3092=LINE('',#18323,#4245);
#3093=LINE('',#18327,#4246);
#3094=LINE('',#18329,#4247);
#3095=LINE('',#18331,#4248);
#3096=LINE('',#18333,#4249);
#3097=LINE('',#18335,#4250);
#3098=LINE('',#18337,#4251);
#3099=LINE('',#18339,#4252);
#3100=LINE('',#18341,#4253);
#3101=LINE('',#18345,#4254);
#3102=LINE('',#18347,#4255);
#3103=LINE('',#18349,#4256);
#3104=LINE('',#18351,#4257);
#3105=LINE('',#18353,#4258);
#3106=LINE('',#18355,#4259);
#3107=LINE('',#18357,#4260);
#3108=LINE('',#18359,#4261);
#3109=LINE('',#18363,#4262);
#3110=LINE('',#18366,#4263);
#3111=LINE('',#18369,#4264);
#3112=LINE('',#18372,#4265);
#3113=LINE('',#18375,#4266);
#3114=LINE('',#18378,#4267);
#3115=LINE('',#18381,#4268);
#3116=LINE('',#18383,#4269);
#3117=LINE('',#18387,#4270);
#3118=LINE('',#18389,#4271);
#3119=LINE('',#18393,#4272);
#3120=LINE('',#18395,#4273);
#3121=LINE('',#18399,#4274);
#3122=LINE('',#18401,#4275);
#3123=LINE('',#18403,#4276);
#3124=LINE('',#18405,#4277);
#3125=LINE('',#18407,#4278);
#3126=LINE('',#18409,#4279);
#3127=LINE('',#18411,#4280);
#3128=LINE('',#18413,#4281);
#3129=LINE('',#18414,#4282);
#3130=LINE('',#18416,#4283);
#3131=LINE('',#18418,#4284);
#3132=LINE('',#18420,#4285);
#3133=LINE('',#18422,#4286);
#3134=LINE('',#18424,#4287);
#3135=LINE('',#18426,#4288);
#3136=LINE('',#18428,#4289);
#3137=LINE('',#18429,#4290);
#3138=LINE('',#18431,#4291);
#3139=LINE('',#18433,#4292);
#3140=LINE('',#18435,#4293);
#3141=LINE('',#18437,#4294);
#3142=LINE('',#18439,#4295);
#3143=LINE('',#18441,#4296);
#3144=LINE('',#18443,#4297);
#3145=LINE('',#18444,#4298);
#3146=LINE('',#18446,#4299);
#3147=LINE('',#18448,#4300);
#3148=LINE('',#18450,#4301);
#3149=LINE('',#18452,#4302);
#3150=LINE('',#18454,#4303);
#3151=LINE('',#18456,#4304);
#3152=LINE('',#18458,#4305);
#3153=LINE('',#18459,#4306);
#3154=LINE('',#18461,#4307);
#3155=LINE('',#18463,#4308);
#3156=LINE('',#18465,#4309);
#3157=LINE('',#18467,#4310);
#3158=LINE('',#18469,#4311);
#3159=LINE('',#18471,#4312);
#3160=LINE('',#18473,#4313);
#3161=LINE('',#18474,#4314);
#3162=LINE('',#18476,#4315);
#3163=LINE('',#18478,#4316);
#3164=LINE('',#18480,#4317);
#3165=LINE('',#18482,#4318);
#3166=LINE('',#18484,#4319);
#3167=LINE('',#18486,#4320);
#3168=LINE('',#18487,#4321);
#3169=LINE('',#18490,#4322);
#3170=LINE('',#18492,#4323);
#3171=LINE('',#18494,#4324);
#3172=LINE('',#18496,#4325);
#3173=LINE('',#18497,#4326);
#3174=LINE('',#18500,#4327);
#3175=LINE('',#18501,#4328);
#3176=LINE('',#18504,#4329);
#3177=LINE('',#18505,#4330);
#3178=LINE('',#18508,#4331);
#3179=LINE('',#18509,#4332);
#3180=LINE('',#18512,#4333);
#3181=LINE('',#18513,#4334);
#3182=LINE('',#18516,#4335);
#3183=LINE('',#18517,#4336);
#3184=LINE('',#18520,#4337);
#3185=LINE('',#18521,#4338);
#3186=LINE('',#18524,#4339);
#3187=LINE('',#18525,#4340);
#3188=LINE('',#18529,#4341);
#3189=LINE('',#18531,#4342);
#3190=LINE('',#18533,#4343);
#3191=LINE('',#18535,#4344);
#3192=LINE('',#18537,#4345);
#3193=LINE('',#18538,#4346);
#3194=LINE('',#18540,#4347);
#3195=LINE('',#18542,#4348);
#3196=LINE('',#18544,#4349);
#3197=LINE('',#18546,#4350);
#3198=LINE('',#18548,#4351);
#3199=LINE('',#18549,#4352);
#3200=LINE('',#18551,#4353);
#3201=LINE('',#18552,#4354);
#3202=LINE('',#18554,#4355);
#3203=LINE('',#18556,#4356);
#3204=LINE('',#18558,#4357);
#3205=LINE('',#18562,#4358);
#3206=LINE('',#18563,#4359);
#3207=LINE('',#18566,#4360);
#3208=LINE('',#18567,#4361);
#3209=LINE('',#18570,#4362);
#3210=LINE('',#18571,#4363);
#3211=LINE('',#18574,#4364);
#3212=LINE('',#18575,#4365);
#3213=LINE('',#18578,#4366);
#3214=LINE('',#18579,#4367);
#3215=LINE('',#18582,#4368);
#3216=LINE('',#18583,#4369);
#3217=LINE('',#18585,#4370);
#3218=LINE('',#18589,#4371);
#3219=LINE('',#18591,#4372);
#3220=LINE('',#18593,#4373);
#3221=LINE('',#18595,#4374);
#3222=LINE('',#18596,#4375);
#3223=LINE('',#18599,#4376);
#3224=LINE('',#18600,#4377);
#3225=LINE('',#18603,#4378);
#3226=LINE('',#18604,#4379);
#3227=LINE('',#18607,#4380);
#3228=LINE('',#18608,#4381);
#3229=LINE('',#18611,#4382);
#3230=LINE('',#18612,#4383);
#3231=LINE('',#18615,#4384);
#3232=LINE('',#18616,#4385);
#3233=LINE('',#18619,#4386);
#3234=LINE('',#18620,#4387);
#3235=LINE('',#18623,#4388);
#3236=LINE('',#18624,#4389);
#3237=LINE('',#18628,#4390);
#3238=LINE('',#18630,#4391);
#3239=LINE('',#18632,#4392);
#3240=LINE('',#18634,#4393);
#3241=LINE('',#18636,#4394);
#3242=LINE('',#18637,#4395);
#3243=LINE('',#18639,#4396);
#3244=LINE('',#18641,#4397);
#3245=LINE('',#18643,#4398);
#3246=LINE('',#18645,#4399);
#3247=LINE('',#18647,#4400);
#3248=LINE('',#18648,#4401);
#3249=LINE('',#18650,#4402);
#3250=LINE('',#18651,#4403);
#3251=LINE('',#18653,#4404);
#3252=LINE('',#18655,#4405);
#3253=LINE('',#18657,#4406);
#3254=LINE('',#18661,#4407);
#3255=LINE('',#18662,#4408);
#3256=LINE('',#18665,#4409);
#3257=LINE('',#18666,#4410);
#3258=LINE('',#18669,#4411);
#3259=LINE('',#18670,#4412);
#3260=LINE('',#18673,#4413);
#3261=LINE('',#18674,#4414);
#3262=LINE('',#18677,#4415);
#3263=LINE('',#18678,#4416);
#3264=LINE('',#18681,#4417);
#3265=LINE('',#18682,#4418);
#3266=LINE('',#18684,#4419);
#3267=LINE('',#18688,#4420);
#3268=LINE('',#18690,#4421);
#3269=LINE('',#18692,#4422);
#3270=LINE('',#18694,#4423);
#3271=LINE('',#18695,#4424);
#3272=LINE('',#18698,#4425);
#3273=LINE('',#18699,#4426);
#3274=LINE('',#18702,#4427);
#3275=LINE('',#18703,#4428);
#3276=LINE('',#18706,#4429);
#3277=LINE('',#18707,#4430);
#3278=LINE('',#18710,#4431);
#3279=LINE('',#18711,#4432);
#3280=LINE('',#18714,#4433);
#3281=LINE('',#18715,#4434);
#3282=LINE('',#18718,#4435);
#3283=LINE('',#18719,#4436);
#3284=LINE('',#18722,#4437);
#3285=LINE('',#18723,#4438);
#3286=LINE('',#18727,#4439);
#3287=LINE('',#18729,#4440);
#3288=LINE('',#18731,#4441);
#3289=LINE('',#18733,#4442);
#3290=LINE('',#18735,#4443);
#3291=LINE('',#18736,#4444);
#3292=LINE('',#18738,#4445);
#3293=LINE('',#18740,#4446);
#3294=LINE('',#18742,#4447);
#3295=LINE('',#18744,#4448);
#3296=LINE('',#18746,#4449);
#3297=LINE('',#18747,#4450);
#3298=LINE('',#18749,#4451);
#3299=LINE('',#18750,#4452);
#3300=LINE('',#18752,#4453);
#3301=LINE('',#18754,#4454);
#3302=LINE('',#18756,#4455);
#3303=LINE('',#18760,#4456);
#3304=LINE('',#18761,#4457);
#3305=LINE('',#18764,#4458);
#3306=LINE('',#18765,#4459);
#3307=LINE('',#18768,#4460);
#3308=LINE('',#18769,#4461);
#3309=LINE('',#18772,#4462);
#3310=LINE('',#18773,#4463);
#3311=LINE('',#18776,#4464);
#3312=LINE('',#18777,#4465);
#3313=LINE('',#18780,#4466);
#3314=LINE('',#18781,#4467);
#3315=LINE('',#18783,#4468);
#3316=LINE('',#18787,#4469);
#3317=LINE('',#18789,#4470);
#3318=LINE('',#18791,#4471);
#3319=LINE('',#18793,#4472);
#3320=LINE('',#18794,#4473);
#3321=LINE('',#18797,#4474);
#3322=LINE('',#18798,#4475);
#3323=LINE('',#18801,#4476);
#3324=LINE('',#18802,#4477);
#3325=LINE('',#18805,#4478);
#3326=LINE('',#18806,#4479);
#3327=LINE('',#18809,#4480);
#3328=LINE('',#18810,#4481);
#3329=LINE('',#18813,#4482);
#3330=LINE('',#18814,#4483);
#3331=LINE('',#18817,#4484);
#3332=LINE('',#18818,#4485);
#3333=LINE('',#18821,#4486);
#3334=LINE('',#18822,#4487);
#3335=LINE('',#18826,#4488);
#3336=LINE('',#18828,#4489);
#3337=LINE('',#18830,#4490);
#3338=LINE('',#18832,#4491);
#3339=LINE('',#18834,#4492);
#3340=LINE('',#18835,#4493);
#3341=LINE('',#18837,#4494);
#3342=LINE('',#18839,#4495);
#3343=LINE('',#18841,#4496);
#3344=LINE('',#18843,#4497);
#3345=LINE('',#18845,#4498);
#3346=LINE('',#18846,#4499);
#3347=LINE('',#18848,#4500);
#3348=LINE('',#18849,#4501);
#3349=LINE('',#18851,#4502);
#3350=LINE('',#18853,#4503);
#3351=LINE('',#18855,#4504);
#3352=LINE('',#18859,#4505);
#3353=LINE('',#18860,#4506);
#3354=LINE('',#18863,#4507);
#3355=LINE('',#18864,#4508);
#3356=LINE('',#18867,#4509);
#3357=LINE('',#18868,#4510);
#3358=LINE('',#18871,#4511);
#3359=LINE('',#18872,#4512);
#3360=LINE('',#18875,#4513);
#3361=LINE('',#18876,#4514);
#3362=LINE('',#18879,#4515);
#3363=LINE('',#18880,#4516);
#3364=LINE('',#18882,#4517);
#3365=LINE('',#18886,#4518);
#3366=LINE('',#18888,#4519);
#3367=LINE('',#18890,#4520);
#3368=LINE('',#18892,#4521);
#3369=LINE('',#18893,#4522);
#3370=LINE('',#18896,#4523);
#3371=LINE('',#18897,#4524);
#3372=LINE('',#18900,#4525);
#3373=LINE('',#18901,#4526);
#3374=LINE('',#18904,#4527);
#3375=LINE('',#18905,#4528);
#3376=LINE('',#18908,#4529);
#3377=LINE('',#18909,#4530);
#3378=LINE('',#18912,#4531);
#3379=LINE('',#18913,#4532);
#3380=LINE('',#18916,#4533);
#3381=LINE('',#18917,#4534);
#3382=LINE('',#18920,#4535);
#3383=LINE('',#18921,#4536);
#3384=LINE('',#18925,#4537);
#3385=LINE('',#18927,#4538);
#3386=LINE('',#18929,#4539);
#3387=LINE('',#18931,#4540);
#3388=LINE('',#18933,#4541);
#3389=LINE('',#18934,#4542);
#3390=LINE('',#18936,#4543);
#3391=LINE('',#18938,#4544);
#3392=LINE('',#18940,#4545);
#3393=LINE('',#18942,#4546);
#3394=LINE('',#18944,#4547);
#3395=LINE('',#18945,#4548);
#3396=LINE('',#18947,#4549);
#3397=LINE('',#18948,#4550);
#3398=LINE('',#18950,#4551);
#3399=LINE('',#18952,#4552);
#3400=LINE('',#18954,#4553);
#3401=LINE('',#18958,#4554);
#3402=LINE('',#18959,#4555);
#3403=LINE('',#18962,#4556);
#3404=LINE('',#18963,#4557);
#3405=LINE('',#18966,#4558);
#3406=LINE('',#18967,#4559);
#3407=LINE('',#18970,#4560);
#3408=LINE('',#18971,#4561);
#3409=LINE('',#18974,#4562);
#3410=LINE('',#18975,#4563);
#3411=LINE('',#18978,#4564);
#3412=LINE('',#18979,#4565);
#3413=LINE('',#18981,#4566);
#3414=LINE('',#18985,#4567);
#3415=LINE('',#18987,#4568);
#3416=LINE('',#18989,#4569);
#3417=LINE('',#18991,#4570);
#3418=LINE('',#18992,#4571);
#3419=LINE('',#18995,#4572);
#3420=LINE('',#18996,#4573);
#3421=LINE('',#18999,#4574);
#3422=LINE('',#19000,#4575);
#3423=LINE('',#19003,#4576);
#3424=LINE('',#19004,#4577);
#3425=LINE('',#19007,#4578);
#3426=LINE('',#19008,#4579);
#3427=LINE('',#19011,#4580);
#3428=LINE('',#19012,#4581);
#3429=LINE('',#19015,#4582);
#3430=LINE('',#19016,#4583);
#3431=LINE('',#19019,#4584);
#3432=LINE('',#19020,#4585);
#3433=LINE('',#19024,#4586);
#3434=LINE('',#19026,#4587);
#3435=LINE('',#19028,#4588);
#3436=LINE('',#19030,#4589);
#3437=LINE('',#19032,#4590);
#3438=LINE('',#19033,#4591);
#3439=LINE('',#19035,#4592);
#3440=LINE('',#19037,#4593);
#3441=LINE('',#19039,#4594);
#3442=LINE('',#19041,#4595);
#3443=LINE('',#19043,#4596);
#3444=LINE('',#19044,#4597);
#3445=LINE('',#19046,#4598);
#3446=LINE('',#19047,#4599);
#3447=LINE('',#19049,#4600);
#3448=LINE('',#19051,#4601);
#3449=LINE('',#19053,#4602);
#3450=LINE('',#19057,#4603);
#3451=LINE('',#19058,#4604);
#3452=LINE('',#19061,#4605);
#3453=LINE('',#19062,#4606);
#3454=LINE('',#19065,#4607);
#3455=LINE('',#19066,#4608);
#3456=LINE('',#19069,#4609);
#3457=LINE('',#19070,#4610);
#3458=LINE('',#19073,#4611);
#3459=LINE('',#19074,#4612);
#3460=LINE('',#19077,#4613);
#3461=LINE('',#19078,#4614);
#3462=LINE('',#19080,#4615);
#3463=LINE('',#19089,#4616);
#3464=LINE('',#19091,#4617);
#3465=LINE('',#19093,#4618);
#3466=LINE('',#19094,#4619);
#3467=LINE('',#19098,#4620);
#3468=LINE('',#19104,#4621);
#3469=LINE('',#19105,#4622);
#3470=LINE('',#19106,#4623);
#3471=LINE('',#19112,#4624);
#3472=LINE('',#19115,#4625);
#3473=LINE('',#19118,#4626);
#3474=LINE('',#19119,#4627);
#3475=LINE('',#19123,#4628);
#3476=LINE('',#19125,#4629);
#3477=LINE('',#19126,#4630);
#3478=LINE('',#19129,#4631);
#3479=LINE('',#19134,#4632);
#3480=LINE('',#19135,#4633);
#3481=LINE('',#19136,#4634);
#3482=LINE('',#19141,#4635);
#3483=LINE('',#19148,#4636);
#3484=LINE('',#19150,#4637);
#3485=LINE('',#19152,#4638);
#3486=LINE('',#19153,#4639);
#3487=LINE('',#19156,#4640);
#3488=LINE('',#19158,#4641);
#3489=LINE('',#19159,#4642);
#3490=LINE('',#19162,#4643);
#3491=LINE('',#19164,#4644);
#3492=LINE('',#19165,#4645);
#3493=LINE('',#19168,#4646);
#3494=LINE('',#19170,#4647);
#3495=LINE('',#19171,#4648);
#3496=LINE('',#19174,#4649);
#3497=LINE('',#19176,#4650);
#3498=LINE('',#19177,#4651);
#3499=LINE('',#19179,#4652);
#3500=LINE('',#19180,#4653);
#3501=LINE('',#19188,#4654);
#3502=LINE('',#19192,#4655);
#3503=LINE('',#19196,#4656);
#3504=LINE('',#19205,#4657);
#3505=LINE('',#19209,#4658);
#3506=LINE('',#19213,#4659);
#3507=LINE('',#19220,#4660);
#3508=LINE('',#19224,#4661);
#3509=LINE('',#19228,#4662);
#3510=LINE('',#19233,#4663);
#3511=LINE('',#19235,#4664);
#3512=LINE('',#19237,#4665);
#3513=LINE('',#19238,#4666);
#3514=LINE('',#19241,#4667);
#3515=LINE('',#19243,#4668);
#3516=LINE('',#19244,#4669);
#3517=LINE('',#19247,#4670);
#3518=LINE('',#19249,#4671);
#3519=LINE('',#19250,#4672);
#3520=LINE('',#19253,#4673);
#3521=LINE('',#19255,#4674);
#3522=LINE('',#19256,#4675);
#3523=LINE('',#19259,#4676);
#3524=LINE('',#19261,#4677);
#3525=LINE('',#19262,#4678);
#3526=LINE('',#19264,#4679);
#3527=LINE('',#19265,#4680);
#3528=VECTOR('',#12350,0.21);
#3529=VECTOR('',#12357,0.21);
#3530=VECTOR('',#12364,0.34);
#3531=VECTOR('',#12371,0.34);
#3532=VECTOR('',#12378,0.34);
#3533=VECTOR('',#12385,0.34);
#3534=VECTOR('',#12390,1.);
#3535=VECTOR('',#12391,1.);
#3536=VECTOR('',#12392,1.);
#3537=VECTOR('',#12393,1.);
#3538=VECTOR('',#12396,1.);
#3539=VECTOR('',#12397,1.);
#3540=VECTOR('',#12398,1.);
#3541=VECTOR('',#12401,1.);
#3542=VECTOR('',#12402,1.);
#3543=VECTOR('',#12403,1.);
#3544=VECTOR('',#12406,1.);
#3545=VECTOR('',#12407,1.);
#3546=VECTOR('',#12416,1.);
#3547=VECTOR('',#12417,1.);
#3548=VECTOR('',#12418,1.);
#3549=VECTOR('',#12419,1.);
#3550=VECTOR('',#12422,1.);
#3551=VECTOR('',#12423,1.);
#3552=VECTOR('',#12424,1.);
#3553=VECTOR('',#12427,1.);
#3554=VECTOR('',#12428,1.);
#3555=VECTOR('',#12429,1.);
#3556=VECTOR('',#12432,1.);
#3557=VECTOR('',#12433,1.);
#3558=VECTOR('',#12442,1.);
#3559=VECTOR('',#12443,1.);
#3560=VECTOR('',#12444,1.);
#3561=VECTOR('',#12445,1.);
#3562=VECTOR('',#12448,1.);
#3563=VECTOR('',#12449,1.);
#3564=VECTOR('',#12450,1.);
#3565=VECTOR('',#12453,1.);
#3566=VECTOR('',#12454,1.);
#3567=VECTOR('',#12455,1.);
#3568=VECTOR('',#12458,1.);
#3569=VECTOR('',#12459,1.);
#3570=VECTOR('',#12470,0.425);
#3571=VECTOR('',#12477,0.645);
#3572=VECTOR('',#12490,0.425);
#3573=VECTOR('',#12497,0.645);
#3574=VECTOR('',#12510,0.425);
#3575=VECTOR('',#12517,0.645);
#3576=VECTOR('',#12530,0.425);
#3577=VECTOR('',#12537,0.645);
#3578=VECTOR('',#12550,0.17);
#3579=VECTOR('',#12557,0.17);
#3580=VECTOR('',#12564,0.17);
#3581=VECTOR('',#12571,0.17);
#3582=VECTOR('',#12578,1.11);
#3583=VECTOR('',#12585,0.275);
#3584=VECTOR('',#12592,0.275);
#3585=VECTOR('',#12597,1.);
#3586=VECTOR('',#12598,1.);
#3587=VECTOR('',#12599,1.);
#3588=VECTOR('',#12600,1.);
#3589=VECTOR('',#12603,1.);
#3590=VECTOR('',#12604,1.);
#3591=VECTOR('',#12605,1.);
#3592=VECTOR('',#12608,1.);
#3593=VECTOR('',#12609,1.);
#3594=VECTOR('',#12610,1.);
#3595=VECTOR('',#12611,1.);
#3596=VECTOR('',#12614,1.);
#3597=VECTOR('',#12615,1.);
#3598=VECTOR('',#12616,1.);
#3599=VECTOR('',#12619,1.);
#3600=VECTOR('',#12620,1.);
#3601=VECTOR('',#12621,1.);
#3602=VECTOR('',#12624,1.);
#3603=VECTOR('',#12635,0.125);
#3604=VECTOR('',#12644,0.125);
#3605=VECTOR('',#12653,0.125);
#3606=VECTOR('',#12662,0.125);
#3607=VECTOR('',#12671,1.1);
#3608=VECTOR('',#12682,0.26);
#3609=VECTOR('',#12685,1.);
#3610=VECTOR('',#12686,1.);
#3611=VECTOR('',#12687,1.);
#3612=VECTOR('',#12688,1.);
#3613=VECTOR('',#12691,1.);
#3614=VECTOR('',#12692,1.);
#3615=VECTOR('',#12693,1.);
#3616=VECTOR('',#12696,1.);
#3617=VECTOR('',#12697,1.);
#3618=VECTOR('',#12698,1.);
#3619=VECTOR('',#12701,1.);
#3620=VECTOR('',#12702,1.);
#3621=VECTOR('',#12711,1.);
#3622=VECTOR('',#12712,1.);
#3623=VECTOR('',#12713,1.);
#3624=VECTOR('',#12714,1.);
#3625=VECTOR('',#12717,1.);
#3626=VECTOR('',#12718,1.);
#3627=VECTOR('',#12719,1.);
#3628=VECTOR('',#12722,1.);
#3629=VECTOR('',#12723,1.);
#3630=VECTOR('',#12724,1.);
#3631=VECTOR('',#12727,1.);
#3632=VECTOR('',#12728,1.);
#3633=VECTOR('',#12729,1.);
#3634=VECTOR('',#12732,1.);
#3635=VECTOR('',#12733,1.);
#3636=VECTOR('',#12734,1.);
#3637=VECTOR('',#12737,1.);
#3638=VECTOR('',#12738,1.);
#3639=VECTOR('',#12751,0.275);
#3640=VECTOR('',#12756,0.15);
#3641=VECTOR('',#12765,1.);
#3642=VECTOR('',#12766,1.);
#3643=VECTOR('',#12767,1.);
#3644=VECTOR('',#12768,1.);
#3645=VECTOR('',#12771,1.);
#3646=VECTOR('',#12772,1.);
#3647=VECTOR('',#12773,1.);
#3648=VECTOR('',#12776,1.);
#3649=VECTOR('',#12777,1.);
#3650=VECTOR('',#12778,1.);
#3651=VECTOR('',#12781,1.);
#3652=VECTOR('',#12782,1.);
#3653=VECTOR('',#12783,1.);
#3654=VECTOR('',#12786,1.);
#3655=VECTOR('',#12787,1.);
#3656=VECTOR('',#12788,1.);
#3657=VECTOR('',#12791,1.);
#3658=VECTOR('',#12792,1.);
#3659=VECTOR('',#12805,0.275);
#3660=VECTOR('',#12810,0.15);
#3661=VECTOR('',#12819,1.);
#3662=VECTOR('',#12820,1.);
#3663=VECTOR('',#12821,1.);
#3664=VECTOR('',#12822,1.);
#3665=VECTOR('',#12825,1.);
#3666=VECTOR('',#12826,1.);
#3667=VECTOR('',#12827,1.);
#3668=VECTOR('',#12830,1.);
#3669=VECTOR('',#12831,1.);
#3670=VECTOR('',#12832,1.);
#3671=VECTOR('',#12835,1.);
#3672=VECTOR('',#12836,1.);
#3673=VECTOR('',#12837,1.);
#3674=VECTOR('',#12840,1.);
#3675=VECTOR('',#12841,1.);
#3676=VECTOR('',#12842,1.);
#3677=VECTOR('',#12845,1.);
#3678=VECTOR('',#12846,1.);
#3679=VECTOR('',#12859,0.275);
#3680=VECTOR('',#12864,0.15);
#3681=VECTOR('',#12873,1.);
#3682=VECTOR('',#12874,1.);
#3683=VECTOR('',#12875,1.);
#3684=VECTOR('',#12876,1.);
#3685=VECTOR('',#12879,1.);
#3686=VECTOR('',#12880,1.);
#3687=VECTOR('',#12881,1.);
#3688=VECTOR('',#12884,1.);
#3689=VECTOR('',#12885,1.);
#3690=VECTOR('',#12886,1.);
#3691=VECTOR('',#12889,1.);
#3692=VECTOR('',#12890,1.);
#3693=VECTOR('',#12891,1.);
#3694=VECTOR('',#12894,1.);
#3695=VECTOR('',#12895,1.);
#3696=VECTOR('',#12896,1.);
#3697=VECTOR('',#12899,1.);
#3698=VECTOR('',#12900,1.);
#3699=VECTOR('',#12913,0.275);
#3700=VECTOR('',#12918,0.15);
#3701=VECTOR('',#12929,1.);
#3702=VECTOR('',#12934,1.);
#3703=VECTOR('',#12937,1.);
#3704=VECTOR('',#12940,2.05);
#3705=VECTOR('',#12949,2.05);
#3706=VECTOR('',#12952,1.);
#3707=VECTOR('',#12953,1.);
#3708=VECTOR('',#12958,1.);
#3709=VECTOR('',#12961,1.);
#3710=VECTOR('',#12964,1.);
#3711=VECTOR('',#12971,1.);
#3712=VECTOR('',#12972,1.);
#3713=VECTOR('',#12977,1.);
#3714=VECTOR('',#12980,1.);
#3715=VECTOR('',#12983,1.);
#3716=VECTOR('',#12986,1.);
#3717=VECTOR('',#12989,1.);
#3718=VECTOR('',#12990,1.);
#3719=VECTOR('',#12993,1.);
#3720=VECTOR('',#12994,1.);
#3721=VECTOR('',#12999,1.);
#3722=VECTOR('',#13000,1.);
#3723=VECTOR('',#13003,1.);
#3724=VECTOR('',#13004,1.);
#3725=VECTOR('',#13005,1.);
#3726=VECTOR('',#13006,1.);
#3727=VECTOR('',#13007,1.);
#3728=VECTOR('',#13008,1.);
#3729=VECTOR('',#13009,1.);
#3730=VECTOR('',#13010,1.);
#3731=VECTOR('',#13011,1.);
#3732=VECTOR('',#13012,1.);
#3733=VECTOR('',#13021,1.);
#3734=VECTOR('',#13024,1.);
#3735=VECTOR('',#13033,1.);
#3736=VECTOR('',#13034,1.);
#3737=VECTOR('',#13035,1.);
#3738=VECTOR('',#13036,1.);
#3739=VECTOR('',#13037,1.);
#3740=VECTOR('',#13040,1.);
#3741=VECTOR('',#13041,1.);
#3742=VECTOR('',#13044,1.);
#3743=VECTOR('',#13045,1.);
#3744=VECTOR('',#13046,1.);
#3745=VECTOR('',#13049,1.);
#3746=VECTOR('',#13050,1.);
#3747=VECTOR('',#13051,1.);
#3748=VECTOR('',#13054,1.);
#3749=VECTOR('',#13061,0.65);
#3750=VECTOR('',#13066,0.65);
#3751=VECTOR('',#13069,1.);
#3752=VECTOR('',#13070,1.);
#3753=VECTOR('',#13071,1.);
#3754=VECTOR('',#13074,1.);
#3755=VECTOR('',#13075,1.);
#3756=VECTOR('',#13078,1.);
#3757=VECTOR('',#13079,1.);
#3758=VECTOR('',#13082,1.);
#3759=VECTOR('',#13091,1.8);
#3760=VECTOR('',#13108,0.25);
#3761=VECTOR('',#13111,0.25);
#3762=VECTOR('',#13116,1.65);
#3763=VECTOR('',#13121,0.25);
#3764=VECTOR('',#13124,0.25);
#3765=VECTOR('',#13127,0.25);
#3766=VECTOR('',#13130,0.25);
#3767=VECTOR('',#13143,1.75);
#3768=VECTOR('',#13150,0.6);
#3769=VECTOR('',#13161,0.42);
#3770=VECTOR('',#13168,0.8);
#3771=VECTOR('',#13179,1.);
#3772=VECTOR('',#13180,1.);
#3773=VECTOR('',#13181,1.);
#3774=VECTOR('',#13182,1.);
#3775=VECTOR('',#13185,1.);
#3776=VECTOR('',#13186,1.);
#3777=VECTOR('',#13187,1.);
#3778=VECTOR('',#13190,1.);
#3779=VECTOR('',#13191,1.);
#3780=VECTOR('',#13192,1.);
#3781=VECTOR('',#13195,1.);
#3782=VECTOR('',#13196,1.);
#3783=VECTOR('',#13197,1.);
#3784=VECTOR('',#13200,1.);
#3785=VECTOR('',#13201,1.);
#3786=VECTOR('',#13202,1.);
#3787=VECTOR('',#13205,1.);
#3788=VECTOR('',#13206,1.);
#3789=VECTOR('',#13223,0.625);
#3790=VECTOR('',#13228,0.65);
#3791=VECTOR('',#13233,0.635);
#3792=VECTOR('',#13242,0.41);
#3793=VECTOR('',#13245,0.4);
#3794=VECTOR('',#13250,1.);
#3795=VECTOR('',#13251,1.);
#3796=VECTOR('',#13252,1.);
#3797=VECTOR('',#13253,1.);
#3798=VECTOR('',#13256,1.);
#3799=VECTOR('',#13257,1.);
#3800=VECTOR('',#13258,1.);
#3801=VECTOR('',#13261,1.);
#3802=VECTOR('',#13262,1.);
#3803=VECTOR('',#13263,1.);
#3804=VECTOR('',#13266,1.);
#3805=VECTOR('',#13267,1.);
#3806=VECTOR('',#13268,1.);
#3807=VECTOR('',#13271,1.);
#3808=VECTOR('',#13272,1.);
#3809=VECTOR('',#13273,1.);
#3810=VECTOR('',#13276,1.);
#3811=VECTOR('',#13277,1.);
#3812=VECTOR('',#13294,0.4);
#3813=VECTOR('',#13299,0.425);
#3814=VECTOR('',#13304,0.41);
#3815=VECTOR('',#13313,0.26);
#3816=VECTOR('',#13316,0.25);
#3817=VECTOR('',#13373,1.);
#3818=VECTOR('',#13374,1.);
#3819=VECTOR('',#13375,1.);
#3820=VECTOR('',#13376,1.);
#3821=VECTOR('',#13381,1.);
#3822=VECTOR('',#13382,1.);
#3823=VECTOR('',#13385,1.);
#3824=VECTOR('',#13386,1.);
#3825=VECTOR('',#13387,1.);
#3826=VECTOR('',#13390,1.);
#3827=VECTOR('',#13399,0.165);
#3828=VECTOR('',#13408,0.6);
#3829=VECTOR('',#13421,0.25);
#3830=VECTOR('',#13432,1.);
#3831=VECTOR('',#13439,0.165);
#3832=VECTOR('',#13444,1.);
#3833=VECTOR('',#13449,0.25);
#3834=VECTOR('',#13456,0.6);
#3835=VECTOR('',#13467,1.);
#3836=VECTOR('',#13474,0.21);
#3837=VECTOR('',#13479,1.);
#3838=VECTOR('',#13482,1.);
#3839=VECTOR('',#13483,1.);
#3840=VECTOR('',#13484,1.);
#3841=VECTOR('',#13485,1.);
#3842=VECTOR('',#13488,1.);
#3843=VECTOR('',#13489,1.);
#3844=VECTOR('',#13490,1.);
#3845=VECTOR('',#13493,1.);
#3846=VECTOR('',#13494,1.);
#3847=VECTOR('',#13495,1.);
#3848=VECTOR('',#13520,2.8);
#3849=VECTOR('',#13523,1.2);
#3850=VECTOR('',#13528,1.2);
#3851=VECTOR('',#13535,1.);
#3852=VECTOR('',#13542,0.21);
#3853=VECTOR('',#13547,1.);
#3854=VECTOR('',#13552,0.605);
#3855=VECTOR('',#13559,1.1);
#3856=VECTOR('',#13570,1.);
#3857=VECTOR('',#13577,0.21);
#3858=VECTOR('',#13582,1.);
#3859=VECTOR('',#13587,0.605);
#3860=VECTOR('',#13594,1.1);
#3861=VECTOR('',#13607,0.225);
#3862=VECTOR('',#13614,0.8);
#3863=VECTOR('',#13625,1.);
#3864=VECTOR('',#13626,1.);
#3865=VECTOR('',#13627,1.);
#3866=VECTOR('',#13628,1.);
#3867=VECTOR('',#13631,1.);
#3868=VECTOR('',#13632,1.);
#3869=VECTOR('',#13633,1.);
#3870=VECTOR('',#13636,1.);
#3871=VECTOR('',#13637,1.);
#3872=VECTOR('',#13638,1.);
#3873=VECTOR('',#13641,1.);
#3874=VECTOR('',#13642,1.);
#3875=VECTOR('',#13643,1.);
#3876=VECTOR('',#13646,1.);
#3877=VECTOR('',#13647,1.);
#3878=VECTOR('',#13648,1.);
#3879=VECTOR('',#13651,1.);
#3880=VECTOR('',#13652,1.);
#3881=VECTOR('',#13663,0.185);
#3882=VECTOR('',#13668,0.2);
#3883=VECTOR('',#13673,0.1625);
#3884=VECTOR('',#13682,0.21);
#3885=VECTOR('',#13687,0.6);
#3886=VECTOR('',#13692,1.);
#3887=VECTOR('',#13693,1.);
#3888=VECTOR('',#13694,1.);
#3889=VECTOR('',#13695,1.);
#3890=VECTOR('',#13698,1.);
#3891=VECTOR('',#13699,1.);
#3892=VECTOR('',#13700,1.);
#3893=VECTOR('',#13703,1.);
#3894=VECTOR('',#13704,1.);
#3895=VECTOR('',#13705,1.);
#3896=VECTOR('',#13708,1.);
#3897=VECTOR('',#13709,1.);
#3898=VECTOR('',#13710,1.);
#3899=VECTOR('',#13713,1.);
#3900=VECTOR('',#13714,1.);
#3901=VECTOR('',#13715,1.);
#3902=VECTOR('',#13718,1.);
#3903=VECTOR('',#13719,1.);
#3904=VECTOR('',#13720,1.);
#3905=VECTOR('',#13723,1.);
#3906=VECTOR('',#13724,1.);
#3907=VECTOR('',#13725,1.);
#3908=VECTOR('',#13728,1.);
#3909=VECTOR('',#13729,1.);
#3910=VECTOR('',#13730,1.);
#3911=VECTOR('',#13733,1.);
#3912=VECTOR('',#13734,1.);
#3913=VECTOR('',#13735,1.);
#3914=VECTOR('',#13738,1.);
#3915=VECTOR('',#13739,1.);
#3916=VECTOR('',#13740,1.);
#3917=VECTOR('',#13743,1.);
#3918=VECTOR('',#13744,1.);
#3919=VECTOR('',#13745,1.);
#3920=VECTOR('',#13748,1.);
#3921=VECTOR('',#13749,1.);
#3922=VECTOR('',#13750,1.);
#3923=VECTOR('',#13753,1.);
#3924=VECTOR('',#13754,1.);
#3925=VECTOR('',#13755,1.);
#3926=VECTOR('',#13758,1.);
#3927=VECTOR('',#13759,1.);
#3928=VECTOR('',#13760,1.);
#3929=VECTOR('',#13763,1.);
#3930=VECTOR('',#13764,1.);
#3931=VECTOR('',#13765,1.);
#3932=VECTOR('',#13768,1.);
#3933=VECTOR('',#13769,1.);
#3934=VECTOR('',#13770,1.);
#3935=VECTOR('',#13773,1.);
#3936=VECTOR('',#13774,1.);
#3937=VECTOR('',#13775,1.);
#3938=VECTOR('',#13778,1.);
#3939=VECTOR('',#13779,1.);
#3940=VECTOR('',#13818,1.);
#3941=VECTOR('',#13819,1.);
#3942=VECTOR('',#13820,1.);
#3943=VECTOR('',#13821,1.);
#3944=VECTOR('',#13822,1.);
#3945=VECTOR('',#13823,1.);
#3946=VECTOR('',#13824,1.);
#3947=VECTOR('',#13825,1.);
#3948=VECTOR('',#13826,1.);
#3949=VECTOR('',#13827,1.);
#3950=VECTOR('',#13830,1.);
#3951=VECTOR('',#13831,1.);
#3952=VECTOR('',#13832,1.);
#3953=VECTOR('',#13833,1.);
#3954=VECTOR('',#13834,1.);
#3955=VECTOR('',#13835,1.);
#3956=VECTOR('',#13836,1.);
#3957=VECTOR('',#13837,1.);
#3958=VECTOR('',#13838,1.);
#3959=VECTOR('',#13839,1.);
#3960=VECTOR('',#13846,1.);
#3961=VECTOR('',#13847,1.);
#3962=VECTOR('',#13848,1.);
#3963=VECTOR('',#13849,1.);
#3964=VECTOR('',#13852,1.);
#3965=VECTOR('',#13853,1.);
#3966=VECTOR('',#13854,1.);
#3967=VECTOR('',#13857,1.);
#3968=VECTOR('',#13858,1.);
#3969=VECTOR('',#13859,1.);
#3970=VECTOR('',#13862,1.);
#3971=VECTOR('',#13863,1.);
#3972=VECTOR('',#13864,1.);
#3973=VECTOR('',#13867,1.);
#3974=VECTOR('',#13868,1.);
#3975=VECTOR('',#13869,1.);
#3976=VECTOR('',#13872,1.);
#3977=VECTOR('',#13873,1.);
#3978=VECTOR('',#13874,1.);
#3979=VECTOR('',#13877,1.);
#3980=VECTOR('',#13878,1.);
#3981=VECTOR('',#13879,1.);
#3982=VECTOR('',#13882,1.);
#3983=VECTOR('',#13883,1.);
#3984=VECTOR('',#13884,1.);
#3985=VECTOR('',#13887,1.);
#3986=VECTOR('',#13888,1.);
#3987=VECTOR('',#13891,1.);
#3988=VECTOR('',#13892,1.);
#3989=VECTOR('',#13895,1.);
#3990=VECTOR('',#13896,1.);
#3991=VECTOR('',#13899,1.);
#3992=VECTOR('',#13900,1.);
#3993=VECTOR('',#13903,1.);
#3994=VECTOR('',#13904,1.);
#3995=VECTOR('',#13907,1.);
#3996=VECTOR('',#13908,1.);
#3997=VECTOR('',#13911,1.);
#3998=VECTOR('',#13912,1.);
#3999=VECTOR('',#13915,1.);
#4000=VECTOR('',#13916,1.);
#4001=VECTOR('',#13919,1.);
#4002=VECTOR('',#13920,1.);
#4003=VECTOR('',#13923,1.);
#4004=VECTOR('',#13960,1.);
#4005=VECTOR('',#13961,1.);
#4006=VECTOR('',#13962,1.);
#4007=VECTOR('',#13963,1.);
#4008=VECTOR('',#13966,1.);
#4009=VECTOR('',#13967,1.);
#4010=VECTOR('',#13968,1.);
#4011=VECTOR('',#13971,1.);
#4012=VECTOR('',#13972,1.);
#4013=VECTOR('',#13973,1.);
#4014=VECTOR('',#13976,1.);
#4015=VECTOR('',#13977,1.);
#4016=VECTOR('',#13978,1.);
#4017=VECTOR('',#13981,1.);
#4018=VECTOR('',#13982,1.);
#4019=VECTOR('',#13983,1.);
#4020=VECTOR('',#13986,1.);
#4021=VECTOR('',#13987,1.);
#4022=VECTOR('',#13988,1.);
#4023=VECTOR('',#13991,1.);
#4024=VECTOR('',#13992,1.);
#4025=VECTOR('',#13993,1.);
#4026=VECTOR('',#13996,1.);
#4027=VECTOR('',#13997,1.);
#4028=VECTOR('',#13998,1.);
#4029=VECTOR('',#14001,1.);
#4030=VECTOR('',#14002,1.);
#4031=VECTOR('',#14005,1.);
#4032=VECTOR('',#14006,1.);
#4033=VECTOR('',#14009,1.);
#4034=VECTOR('',#14010,1.);
#4035=VECTOR('',#14013,1.);
#4036=VECTOR('',#14014,1.);
#4037=VECTOR('',#14017,1.);
#4038=VECTOR('',#14018,1.);
#4039=VECTOR('',#14021,1.);
#4040=VECTOR('',#14022,1.);
#4041=VECTOR('',#14025,1.);
#4042=VECTOR('',#14026,1.);
#4043=VECTOR('',#14029,1.);
#4044=VECTOR('',#14030,1.);
#4045=VECTOR('',#14033,1.);
#4046=VECTOR('',#14034,1.);
#4047=VECTOR('',#14037,1.);
#4048=VECTOR('',#14076,1.37);
#4049=VECTOR('',#14083,0.21);
#4050=VECTOR('',#14088,0.6);
#4051=VECTOR('',#14093,1.);
#4052=VECTOR('',#14094,1.);
#4053=VECTOR('',#14095,1.);
#4054=VECTOR('',#14096,1.);
#4055=VECTOR('',#14099,1.);
#4056=VECTOR('',#14100,1.);
#4057=VECTOR('',#14101,1.);
#4058=VECTOR('',#14104,1.);
#4059=VECTOR('',#14105,1.);
#4060=VECTOR('',#14106,1.);
#4061=VECTOR('',#14109,1.);
#4062=VECTOR('',#14110,1.);
#4063=VECTOR('',#14111,1.);
#4064=VECTOR('',#14114,1.);
#4065=VECTOR('',#14115,1.);
#4066=VECTOR('',#14116,1.);
#4067=VECTOR('',#14119,1.);
#4068=VECTOR('',#14120,1.);
#4069=VECTOR('',#14121,1.);
#4070=VECTOR('',#14124,1.);
#4071=VECTOR('',#14125,1.);
#4072=VECTOR('',#14126,1.);
#4073=VECTOR('',#14129,1.);
#4074=VECTOR('',#14130,1.);
#4075=VECTOR('',#14131,1.);
#4076=VECTOR('',#14134,1.);
#4077=VECTOR('',#14135,1.);
#4078=VECTOR('',#14136,1.);
#4079=VECTOR('',#14139,1.);
#4080=VECTOR('',#14140,1.);
#4081=VECTOR('',#14141,1.);
#4082=VECTOR('',#14144,1.);
#4083=VECTOR('',#14145,1.);
#4084=VECTOR('',#14146,1.);
#4085=VECTOR('',#14149,1.);
#4086=VECTOR('',#14150,1.);
#4087=VECTOR('',#14151,1.);
#4088=VECTOR('',#14154,1.);
#4089=VECTOR('',#14155,1.);
#4090=VECTOR('',#14156,1.);
#4091=VECTOR('',#14159,1.);
#4092=VECTOR('',#14160,1.);
#4093=VECTOR('',#14161,1.);
#4094=VECTOR('',#14164,1.);
#4095=VECTOR('',#14165,1.);
#4096=VECTOR('',#14166,1.);
#4097=VECTOR('',#14169,1.);
#4098=VECTOR('',#14170,1.);
#4099=VECTOR('',#14171,1.);
#4100=VECTOR('',#14174,1.);
#4101=VECTOR('',#14175,1.);
#4102=VECTOR('',#14176,1.);
#4103=VECTOR('',#14179,1.);
#4104=VECTOR('',#14180,1.);
#4105=VECTOR('',#14213,1.);
#4106=VECTOR('',#14214,1.);
#4107=VECTOR('',#14215,1.);
#4108=VECTOR('',#14216,1.);
#4109=VECTOR('',#14217,1.);
#4110=VECTOR('',#14218,1.);
#4111=VECTOR('',#14219,1.);
#4112=VECTOR('',#14220,1.);
#4113=VECTOR('',#14221,1.);
#4114=VECTOR('',#14222,1.);
#4115=VECTOR('',#14225,1.);
#4116=VECTOR('',#14226,1.);
#4117=VECTOR('',#14227,1.);
#4118=VECTOR('',#14228,1.);
#4119=VECTOR('',#14229,1.);
#4120=VECTOR('',#14230,1.);
#4121=VECTOR('',#14231,1.);
#4122=VECTOR('',#14232,1.);
#4123=VECTOR('',#14233,1.);
#4124=VECTOR('',#14234,1.);
#4125=VECTOR('',#14247,1.);
#4126=VECTOR('',#14248,1.);
#4127=VECTOR('',#14249,1.);
#4128=VECTOR('',#14252,1.);
#4129=VECTOR('',#14253,1.);
#4130=VECTOR('',#14256,1.);
#4131=VECTOR('',#14257,1.);
#4132=VECTOR('',#14260,1.);
#4133=VECTOR('',#14261,1.);
#4134=VECTOR('',#14264,1.);
#4135=VECTOR('',#14265,1.);
#4136=VECTOR('',#14268,1.);
#4137=VECTOR('',#14269,1.);
#4138=VECTOR('',#14272,1.);
#4139=VECTOR('',#14273,1.);
#4140=VECTOR('',#14276,1.);
#4141=VECTOR('',#14277,1.);
#4142=VECTOR('',#14280,1.);
#4143=VECTOR('',#14281,1.);
#4144=VECTOR('',#14284,1.);
#4145=VECTOR('',#14285,1.);
#4146=VECTOR('',#14286,1.);
#4147=VECTOR('',#14289,1.);
#4148=VECTOR('',#14290,1.);
#4149=VECTOR('',#14291,1.);
#4150=VECTOR('',#14294,1.);
#4151=VECTOR('',#14295,1.);
#4152=VECTOR('',#14296,1.);
#4153=VECTOR('',#14299,1.);
#4154=VECTOR('',#14300,1.);
#4155=VECTOR('',#14301,1.);
#4156=VECTOR('',#14304,1.);
#4157=VECTOR('',#14305,1.);
#4158=VECTOR('',#14306,1.);
#4159=VECTOR('',#14309,1.);
#4160=VECTOR('',#14310,1.);
#4161=VECTOR('',#14311,1.);
#4162=VECTOR('',#14314,1.);
#4163=VECTOR('',#14315,1.);
#4164=VECTOR('',#14316,1.);
#4165=VECTOR('',#14319,1.);
#4166=VECTOR('',#14320,1.);
#4167=VECTOR('',#14321,1.);
#4168=VECTOR('',#14324,1.);
#4169=VECTOR('',#14361,1.);
#4170=VECTOR('',#14362,1.);
#4171=VECTOR('',#14363,1.);
#4172=VECTOR('',#14366,1.);
#4173=VECTOR('',#14367,1.);
#4174=VECTOR('',#14370,1.);
#4175=VECTOR('',#14371,1.);
#4176=VECTOR('',#14374,1.);
#4177=VECTOR('',#14375,1.);
#4178=VECTOR('',#14378,1.);
#4179=VECTOR('',#14379,1.);
#4180=VECTOR('',#14382,1.);
#4181=VECTOR('',#14383,1.);
#4182=VECTOR('',#14386,1.);
#4183=VECTOR('',#14387,1.);
#4184=VECTOR('',#14390,1.);
#4185=VECTOR('',#14391,1.);
#4186=VECTOR('',#14394,1.);
#4187=VECTOR('',#14395,1.);
#4188=VECTOR('',#14398,1.);
#4189=VECTOR('',#14399,1.);
#4190=VECTOR('',#14400,1.);
#4191=VECTOR('',#14403,1.);
#4192=VECTOR('',#14404,1.);
#4193=VECTOR('',#14405,1.);
#4194=VECTOR('',#14408,1.);
#4195=VECTOR('',#14409,1.);
#4196=VECTOR('',#14410,1.);
#4197=VECTOR('',#14413,1.);
#4198=VECTOR('',#14414,1.);
#4199=VECTOR('',#14415,1.);
#4200=VECTOR('',#14418,1.);
#4201=VECTOR('',#14419,1.);
#4202=VECTOR('',#14420,1.);
#4203=VECTOR('',#14423,1.);
#4204=VECTOR('',#14424,1.);
#4205=VECTOR('',#14425,1.);
#4206=VECTOR('',#14428,1.);
#4207=VECTOR('',#14429,1.);
#4208=VECTOR('',#14430,1.);
#4209=VECTOR('',#14433,1.);
#4210=VECTOR('',#14434,1.);
#4211=VECTOR('',#14435,1.);
#4212=VECTOR('',#14438,1.);
#4213=VECTOR('',#14477,1.37);
#4214=VECTOR('',#14484,1.);
#4215=VECTOR('',#14485,1.);
#4216=VECTOR('',#14486,1.);
#4217=VECTOR('',#14487,1.);
#4218=VECTOR('',#14488,1.);
#4219=VECTOR('',#14489,1.);
#4220=VECTOR('',#14490,1.);
#4221=VECTOR('',#14491,1.);
#4222=VECTOR('',#14494,1.);
#4223=VECTOR('',#14495,1.);
#4224=VECTOR('',#14496,1.);
#4225=VECTOR('',#14497,1.);
#4226=VECTOR('',#14498,1.);
#4227=VECTOR('',#14499,1.);
#4228=VECTOR('',#14500,1.);
#4229=VECTOR('',#14501,1.);
#4230=VECTOR('',#14504,1.);
#4231=VECTOR('',#14505,1.);
#4232=VECTOR('',#14506,1.);
#4233=VECTOR('',#14507,1.);
#4234=VECTOR('',#14508,1.);
#4235=VECTOR('',#14509,1.);
#4236=VECTOR('',#14510,1.);
#4237=VECTOR('',#14511,1.);
#4238=VECTOR('',#14514,1.);
#4239=VECTOR('',#14515,1.);
#4240=VECTOR('',#14516,1.);
#4241=VECTOR('',#14517,1.);
#4242=VECTOR('',#14518,1.);
#4243=VECTOR('',#14519,1.);
#4244=VECTOR('',#14520,1.);
#4245=VECTOR('',#14521,1.);
#4246=VECTOR('',#14524,1.);
#4247=VECTOR('',#14525,1.);
#4248=VECTOR('',#14526,1.);
#4249=VECTOR('',#14527,1.);
#4250=VECTOR('',#14528,1.);
#4251=VECTOR('',#14529,1.);
#4252=VECTOR('',#14530,1.);
#4253=VECTOR('',#14531,1.);
#4254=VECTOR('',#14534,1.);
#4255=VECTOR('',#14535,1.);
#4256=VECTOR('',#14536,1.);
#4257=VECTOR('',#14537,1.);
#4258=VECTOR('',#14538,1.);
#4259=VECTOR('',#14539,1.);
#4260=VECTOR('',#14540,1.);
#4261=VECTOR('',#14541,1.);
#4262=VECTOR('',#14546,1.);
#4263=VECTOR('',#14549,1.);
#4264=VECTOR('',#14552,1.);
#4265=VECTOR('',#14555,1.);
#4266=VECTOR('',#14558,1.);
#4267=VECTOR('',#14561,1.);
#4268=VECTOR('',#14564,1.);
#4269=VECTOR('',#14565,1.);
#4270=VECTOR('',#14570,1.);
#4271=VECTOR('',#14571,1.);
#4272=VECTOR('',#14576,1.);
#4273=VECTOR('',#14577,1.);
#4274=VECTOR('',#14582,1.);
#4275=VECTOR('',#14583,1.);
#4276=VECTOR('',#14584,1.);
#4277=VECTOR('',#14585,1.);
#4278=VECTOR('',#14586,1.);
#4279=VECTOR('',#14587,1.);
#4280=VECTOR('',#14588,1.);
#4281=VECTOR('',#14589,1.);
#4282=VECTOR('',#14590,1.);
#4283=VECTOR('',#14591,1.);
#4284=VECTOR('',#14592,1.);
#4285=VECTOR('',#14593,1.);
#4286=VECTOR('',#14594,1.);
#4287=VECTOR('',#14595,1.);
#4288=VECTOR('',#14596,1.);
#4289=VECTOR('',#14597,1.);
#4290=VECTOR('',#14598,1.);
#4291=VECTOR('',#14599,1.);
#4292=VECTOR('',#14600,1.);
#4293=VECTOR('',#14601,1.);
#4294=VECTOR('',#14602,1.);
#4295=VECTOR('',#14603,1.);
#4296=VECTOR('',#14604,1.);
#4297=VECTOR('',#14605,1.);
#4298=VECTOR('',#14606,1.);
#4299=VECTOR('',#14607,1.);
#4300=VECTOR('',#14608,1.);
#4301=VECTOR('',#14609,1.);
#4302=VECTOR('',#14610,1.);
#4303=VECTOR('',#14611,1.);
#4304=VECTOR('',#14612,1.);
#4305=VECTOR('',#14613,1.);
#4306=VECTOR('',#14614,1.);
#4307=VECTOR('',#14615,1.);
#4308=VECTOR('',#14616,1.);
#4309=VECTOR('',#14617,1.);
#4310=VECTOR('',#14618,1.);
#4311=VECTOR('',#14619,1.);
#4312=VECTOR('',#14620,1.);
#4313=VECTOR('',#14621,1.);
#4314=VECTOR('',#14622,1.);
#4315=VECTOR('',#14623,1.);
#4316=VECTOR('',#14624,1.);
#4317=VECTOR('',#14625,1.);
#4318=VECTOR('',#14626,1.);
#4319=VECTOR('',#14627,1.);
#4320=VECTOR('',#14628,1.);
#4321=VECTOR('',#14629,1.);
#4322=VECTOR('',#14632,1.);
#4323=VECTOR('',#14633,1.);
#4324=VECTOR('',#14634,1.);
#4325=VECTOR('',#14635,1.);
#4326=VECTOR('',#14636,1.);
#4327=VECTOR('',#14639,1.);
#4328=VECTOR('',#14640,1.);
#4329=VECTOR('',#14643,1.);
#4330=VECTOR('',#14644,1.);
#4331=VECTOR('',#14647,1.);
#4332=VECTOR('',#14648,1.);
#4333=VECTOR('',#14651,1.);
#4334=VECTOR('',#14652,1.);
#4335=VECTOR('',#14655,1.);
#4336=VECTOR('',#14656,1.);
#4337=VECTOR('',#14659,1.);
#4338=VECTOR('',#14660,1.);
#4339=VECTOR('',#14663,1.);
#4340=VECTOR('',#14664,1.);
#4341=VECTOR('',#14667,1.);
#4342=VECTOR('',#14668,1.);
#4343=VECTOR('',#14669,1.);
#4344=VECTOR('',#14670,1.);
#4345=VECTOR('',#14671,1.);
#4346=VECTOR('',#14672,1.);
#4347=VECTOR('',#14673,1.);
#4348=VECTOR('',#14674,1.);
#4349=VECTOR('',#14675,1.);
#4350=VECTOR('',#14676,1.);
#4351=VECTOR('',#14677,1.);
#4352=VECTOR('',#14678,1.);
#4353=VECTOR('',#14681,1.);
#4354=VECTOR('',#14682,1.);
#4355=VECTOR('',#14685,1.);
#4356=VECTOR('',#14688,1.);
#4357=VECTOR('',#14691,1.);
#4358=VECTOR('',#14696,1.);
#4359=VECTOR('',#14697,1.);
#4360=VECTOR('',#14700,1.);
#4361=VECTOR('',#14701,1.);
#4362=VECTOR('',#14704,1.);
#4363=VECTOR('',#14705,1.);
#4364=VECTOR('',#14708,1.);
#4365=VECTOR('',#14709,1.);
#4366=VECTOR('',#14712,1.);
#4367=VECTOR('',#14713,1.);
#4368=VECTOR('',#14716,1.);
#4369=VECTOR('',#14717,1.);
#4370=VECTOR('',#14720,1.);
#4371=VECTOR('',#14725,1.);
#4372=VECTOR('',#14726,1.);
#4373=VECTOR('',#14727,1.);
#4374=VECTOR('',#14728,1.);
#4375=VECTOR('',#14729,1.);
#4376=VECTOR('',#14732,1.);
#4377=VECTOR('',#14733,1.);
#4378=VECTOR('',#14736,1.);
#4379=VECTOR('',#14737,1.);
#4380=VECTOR('',#14740,1.);
#4381=VECTOR('',#14741,1.);
#4382=VECTOR('',#14744,1.);
#4383=VECTOR('',#14745,1.);
#4384=VECTOR('',#14748,1.);
#4385=VECTOR('',#14749,1.);
#4386=VECTOR('',#14752,1.);
#4387=VECTOR('',#14753,1.);
#4388=VECTOR('',#14756,1.);
#4389=VECTOR('',#14757,1.);
#4390=VECTOR('',#14760,1.);
#4391=VECTOR('',#14761,1.);
#4392=VECTOR('',#14762,1.);
#4393=VECTOR('',#14763,1.);
#4394=VECTOR('',#14764,1.);
#4395=VECTOR('',#14765,1.);
#4396=VECTOR('',#14766,1.);
#4397=VECTOR('',#14767,1.);
#4398=VECTOR('',#14768,1.);
#4399=VECTOR('',#14769,1.);
#4400=VECTOR('',#14770,1.);
#4401=VECTOR('',#14771,1.);
#4402=VECTOR('',#14774,1.);
#4403=VECTOR('',#14775,1.);
#4404=VECTOR('',#14778,1.);
#4405=VECTOR('',#14781,1.);
#4406=VECTOR('',#14784,1.);
#4407=VECTOR('',#14789,1.);
#4408=VECTOR('',#14790,1.);
#4409=VECTOR('',#14793,1.);
#4410=VECTOR('',#14794,1.);
#4411=VECTOR('',#14797,1.);
#4412=VECTOR('',#14798,1.);
#4413=VECTOR('',#14801,1.);
#4414=VECTOR('',#14802,1.);
#4415=VECTOR('',#14805,1.);
#4416=VECTOR('',#14806,1.);
#4417=VECTOR('',#14809,1.);
#4418=VECTOR('',#14810,1.);
#4419=VECTOR('',#14813,1.);
#4420=VECTOR('',#14818,1.);
#4421=VECTOR('',#14819,1.);
#4422=VECTOR('',#14820,1.);
#4423=VECTOR('',#14821,1.);
#4424=VECTOR('',#14822,1.);
#4425=VECTOR('',#14825,1.);
#4426=VECTOR('',#14826,1.);
#4427=VECTOR('',#14829,1.);
#4428=VECTOR('',#14830,1.);
#4429=VECTOR('',#14833,1.);
#4430=VECTOR('',#14834,1.);
#4431=VECTOR('',#14837,1.);
#4432=VECTOR('',#14838,1.);
#4433=VECTOR('',#14841,1.);
#4434=VECTOR('',#14842,1.);
#4435=VECTOR('',#14845,1.);
#4436=VECTOR('',#14846,1.);
#4437=VECTOR('',#14849,1.);
#4438=VECTOR('',#14850,1.);
#4439=VECTOR('',#14853,1.);
#4440=VECTOR('',#14854,1.);
#4441=VECTOR('',#14855,1.);
#4442=VECTOR('',#14856,1.);
#4443=VECTOR('',#14857,1.);
#4444=VECTOR('',#14858,1.);
#4445=VECTOR('',#14859,1.);
#4446=VECTOR('',#14860,1.);
#4447=VECTOR('',#14861,1.);
#4448=VECTOR('',#14862,1.);
#4449=VECTOR('',#14863,1.);
#4450=VECTOR('',#14864,1.);
#4451=VECTOR('',#14867,1.);
#4452=VECTOR('',#14868,1.);
#4453=VECTOR('',#14871,1.);
#4454=VECTOR('',#14874,1.);
#4455=VECTOR('',#14877,1.);
#4456=VECTOR('',#14882,1.);
#4457=VECTOR('',#14883,1.);
#4458=VECTOR('',#14886,1.);
#4459=VECTOR('',#14887,1.);
#4460=VECTOR('',#14890,1.);
#4461=VECTOR('',#14891,1.);
#4462=VECTOR('',#14894,1.);
#4463=VECTOR('',#14895,1.);
#4464=VECTOR('',#14898,1.);
#4465=VECTOR('',#14899,1.);
#4466=VECTOR('',#14902,1.);
#4467=VECTOR('',#14903,1.);
#4468=VECTOR('',#14906,1.);
#4469=VECTOR('',#14911,1.);
#4470=VECTOR('',#14912,1.);
#4471=VECTOR('',#14913,1.);
#4472=VECTOR('',#14914,1.);
#4473=VECTOR('',#14915,1.);
#4474=VECTOR('',#14918,1.);
#4475=VECTOR('',#14919,1.);
#4476=VECTOR('',#14922,1.);
#4477=VECTOR('',#14923,1.);
#4478=VECTOR('',#14926,1.);
#4479=VECTOR('',#14927,1.);
#4480=VECTOR('',#14930,1.);
#4481=VECTOR('',#14931,1.);
#4482=VECTOR('',#14934,1.);
#4483=VECTOR('',#14935,1.);
#4484=VECTOR('',#14938,1.);
#4485=VECTOR('',#14939,1.);
#4486=VECTOR('',#14942,1.);
#4487=VECTOR('',#14943,1.);
#4488=VECTOR('',#14946,1.);
#4489=VECTOR('',#14947,1.);
#4490=VECTOR('',#14948,1.);
#4491=VECTOR('',#14949,1.);
#4492=VECTOR('',#14950,1.);
#4493=VECTOR('',#14951,1.);
#4494=VECTOR('',#14952,1.);
#4495=VECTOR('',#14953,1.);
#4496=VECTOR('',#14954,1.);
#4497=VECTOR('',#14955,1.);
#4498=VECTOR('',#14956,1.);
#4499=VECTOR('',#14957,1.);
#4500=VECTOR('',#14960,1.);
#4501=VECTOR('',#14961,1.);
#4502=VECTOR('',#14964,1.);
#4503=VECTOR('',#14967,1.);
#4504=VECTOR('',#14970,1.);
#4505=VECTOR('',#14975,1.);
#4506=VECTOR('',#14976,1.);
#4507=VECTOR('',#14979,1.);
#4508=VECTOR('',#14980,1.);
#4509=VECTOR('',#14983,1.);
#4510=VECTOR('',#14984,1.);
#4511=VECTOR('',#14987,1.);
#4512=VECTOR('',#14988,1.);
#4513=VECTOR('',#14991,1.);
#4514=VECTOR('',#14992,1.);
#4515=VECTOR('',#14995,1.);
#4516=VECTOR('',#14996,1.);
#4517=VECTOR('',#14999,1.);
#4518=VECTOR('',#15004,1.);
#4519=VECTOR('',#15005,1.);
#4520=VECTOR('',#15006,1.);
#4521=VECTOR('',#15007,1.);
#4522=VECTOR('',#15008,1.);
#4523=VECTOR('',#15011,1.);
#4524=VECTOR('',#15012,1.);
#4525=VECTOR('',#15015,1.);
#4526=VECTOR('',#15016,1.);
#4527=VECTOR('',#15019,1.);
#4528=VECTOR('',#15020,1.);
#4529=VECTOR('',#15023,1.);
#4530=VECTOR('',#15024,1.);
#4531=VECTOR('',#15027,1.);
#4532=VECTOR('',#15028,1.);
#4533=VECTOR('',#15031,1.);
#4534=VECTOR('',#15032,1.);
#4535=VECTOR('',#15035,1.);
#4536=VECTOR('',#15036,1.);
#4537=VECTOR('',#15039,1.);
#4538=VECTOR('',#15040,1.);
#4539=VECTOR('',#15041,1.);
#4540=VECTOR('',#15042,1.);
#4541=VECTOR('',#15043,1.);
#4542=VECTOR('',#15044,1.);
#4543=VECTOR('',#15045,1.);
#4544=VECTOR('',#15046,1.);
#4545=VECTOR('',#15047,1.);
#4546=VECTOR('',#15048,1.);
#4547=VECTOR('',#15049,1.);
#4548=VECTOR('',#15050,1.);
#4549=VECTOR('',#15053,1.);
#4550=VECTOR('',#15054,1.);
#4551=VECTOR('',#15057,1.);
#4552=VECTOR('',#15060,1.);
#4553=VECTOR('',#15063,1.);
#4554=VECTOR('',#15068,1.);
#4555=VECTOR('',#15069,1.);
#4556=VECTOR('',#15072,1.);
#4557=VECTOR('',#15073,1.);
#4558=VECTOR('',#15076,1.);
#4559=VECTOR('',#15077,1.);
#4560=VECTOR('',#15080,1.);
#4561=VECTOR('',#15081,1.);
#4562=VECTOR('',#15084,1.);
#4563=VECTOR('',#15085,1.);
#4564=VECTOR('',#15088,1.);
#4565=VECTOR('',#15089,1.);
#4566=VECTOR('',#15092,1.);
#4567=VECTOR('',#15097,1.);
#4568=VECTOR('',#15098,1.);
#4569=VECTOR('',#15099,1.);
#4570=VECTOR('',#15100,1.);
#4571=VECTOR('',#15101,1.);
#4572=VECTOR('',#15104,1.);
#4573=VECTOR('',#15105,1.);
#4574=VECTOR('',#15108,1.);
#4575=VECTOR('',#15109,1.);
#4576=VECTOR('',#15112,1.);
#4577=VECTOR('',#15113,1.);
#4578=VECTOR('',#15116,1.);
#4579=VECTOR('',#15117,1.);
#4580=VECTOR('',#15120,1.);
#4581=VECTOR('',#15121,1.);
#4582=VECTOR('',#15124,1.);
#4583=VECTOR('',#15125,1.);
#4584=VECTOR('',#15128,1.);
#4585=VECTOR('',#15129,1.);
#4586=VECTOR('',#15132,1.);
#4587=VECTOR('',#15133,1.);
#4588=VECTOR('',#15134,1.);
#4589=VECTOR('',#15135,1.);
#4590=VECTOR('',#15136,1.);
#4591=VECTOR('',#15137,1.);
#4592=VECTOR('',#15138,1.);
#4593=VECTOR('',#15139,1.);
#4594=VECTOR('',#15140,1.);
#4595=VECTOR('',#15141,1.);
#4596=VECTOR('',#15142,1.);
#4597=VECTOR('',#15143,1.);
#4598=VECTOR('',#15146,1.);
#4599=VECTOR('',#15147,1.);
#4600=VECTOR('',#15150,1.);
#4601=VECTOR('',#15153,1.);
#4602=VECTOR('',#15156,1.);
#4603=VECTOR('',#15161,1.);
#4604=VECTOR('',#15162,1.);
#4605=VECTOR('',#15165,1.);
#4606=VECTOR('',#15166,1.);
#4607=VECTOR('',#15169,1.);
#4608=VECTOR('',#15170,1.);
#4609=VECTOR('',#15173,1.);
#4610=VECTOR('',#15174,1.);
#4611=VECTOR('',#15177,1.);
#4612=VECTOR('',#15178,1.);
#4613=VECTOR('',#15181,1.);
#4614=VECTOR('',#15182,1.);
#4615=VECTOR('',#15185,1.);
#4616=VECTOR('',#15198,1.);
#4617=VECTOR('',#15199,1.);
#4618=VECTOR('',#15200,1.);
#4619=VECTOR('',#15201,1.);
#4620=VECTOR('',#15204,1.);
#4621=VECTOR('',#15211,1.);
#4622=VECTOR('',#15212,1.);
#4623=VECTOR('',#15213,1.);
#4624=VECTOR('',#15222,1.);
#4625=VECTOR('',#15225,1.);
#4626=VECTOR('',#15228,1.);
#4627=VECTOR('',#15229,1.);
#4628=VECTOR('',#15234,1.);
#4629=VECTOR('',#15235,1.);
#4630=VECTOR('',#15236,1.);
#4631=VECTOR('',#15239,1.);
#4632=VECTOR('',#15244,1.);
#4633=VECTOR('',#15245,1.);
#4634=VECTOR('',#15246,1.);
#4635=VECTOR('',#15255,1.);
#4636=VECTOR('',#15264,1.);
#4637=VECTOR('',#15265,1.);
#4638=VECTOR('',#15266,1.);
#4639=VECTOR('',#15267,1.);
#4640=VECTOR('',#15270,1.);
#4641=VECTOR('',#15271,1.);
#4642=VECTOR('',#15272,1.);
#4643=VECTOR('',#15275,1.);
#4644=VECTOR('',#15276,1.);
#4645=VECTOR('',#15277,1.);
#4646=VECTOR('',#15280,1.);
#4647=VECTOR('',#15281,1.);
#4648=VECTOR('',#15282,1.);
#4649=VECTOR('',#15285,1.);
#4650=VECTOR('',#15286,1.);
#4651=VECTOR('',#15287,1.);
#4652=VECTOR('',#15290,1.);
#4653=VECTOR('',#15291,1.);
#4654=VECTOR('',#15302,0.235);
#4655=VECTOR('',#15307,0.25);
#4656=VECTOR('',#15312,0.2125);
#4657=VECTOR('',#15325,0.325);
#4658=VECTOR('',#15330,0.35);
#4659=VECTOR('',#15335,0.335);
#4660=VECTOR('',#15344,0.21);
#4661=VECTOR('',#15349,0.2);
#4662=VECTOR('',#15354,0.18);
#4663=VECTOR('',#15359,1.);
#4664=VECTOR('',#15360,1.);
#4665=VECTOR('',#15361,1.);
#4666=VECTOR('',#15362,1.);
#4667=VECTOR('',#15365,1.);
#4668=VECTOR('',#15366,1.);
#4669=VECTOR('',#15367,1.);
#4670=VECTOR('',#15370,1.);
#4671=VECTOR('',#15371,1.);
#4672=VECTOR('',#15372,1.);
#4673=VECTOR('',#15375,1.);
#4674=VECTOR('',#15376,1.);
#4675=VECTOR('',#15377,1.);
#4676=VECTOR('',#15380,1.);
#4677=VECTOR('',#15381,1.);
#4678=VECTOR('',#15382,1.);
#4679=VECTOR('',#15385,1.);
#4680=VECTOR('',#15386,1.);
#4681=CIRCLE('',#11377,0.21);
#4682=CIRCLE('',#11378,0.21);
#4683=CIRCLE('',#11380,0.21);
#4684=CIRCLE('',#11381,0.21);
#4685=CIRCLE('',#11383,0.34);
#4686=CIRCLE('',#11384,0.34);
#4687=CIRCLE('',#11386,0.34);
#4688=CIRCLE('',#11387,0.34);
#4689=CIRCLE('',#11389,0.34);
#4690=CIRCLE('',#11390,0.34);
#4691=CIRCLE('',#11392,0.34);
#4692=CIRCLE('',#11393,0.34);
#4693=CIRCLE('',#11416,0.425);
#4694=CIRCLE('',#11417,0.425);
#4695=CIRCLE('',#11419,0.645);
#4696=CIRCLE('',#11420,0.645);
#4697=CIRCLE('',#11425,0.425);
#4698=CIRCLE('',#11426,0.425);
#4699=CIRCLE('',#11428,0.645);
#4700=CIRCLE('',#11429,0.645);
#4701=CIRCLE('',#11434,0.425);
#4702=CIRCLE('',#11435,0.425);
#4703=CIRCLE('',#11437,0.645);
#4704=CIRCLE('',#11438,0.645);
#4705=CIRCLE('',#11443,0.425);
#4706=CIRCLE('',#11444,0.425);
#4707=CIRCLE('',#11446,0.645);
#4708=CIRCLE('',#11447,0.645);
#4709=CIRCLE('',#11452,0.17);
#4710=CIRCLE('',#11453,0.17);
#4711=CIRCLE('',#11455,0.17);
#4712=CIRCLE('',#11456,0.17);
#4713=CIRCLE('',#11458,0.17);
#4714=CIRCLE('',#11459,0.17);
#4715=CIRCLE('',#11461,0.17);
#4716=CIRCLE('',#11462,0.17);
#4717=CIRCLE('',#11464,1.11);
#4718=CIRCLE('',#11465,1.11);
#4719=CIRCLE('',#11467,0.275);
#4720=CIRCLE('',#11468,0.275);
#4721=CIRCLE('',#11470,0.275);
#4722=CIRCLE('',#11471,0.275);
#4723=CIRCLE('',#11482,0.125);
#4724=CIRCLE('',#11483,0.125);
#4725=CIRCLE('',#11486,0.125);
#4726=CIRCLE('',#11487,0.125);
#4727=CIRCLE('',#11490,0.125);
#4728=CIRCLE('',#11491,0.125);
#4729=CIRCLE('',#11494,0.125);
#4730=CIRCLE('',#11495,0.125);
#4731=CIRCLE('',#11498,1.1);
#4732=CIRCLE('',#11499,1.1);
#4733=CIRCLE('',#11501,0.26);
#4734=CIRCLE('',#11503,0.26);
#4735=CIRCLE('',#11519,0.275);
#4736=CIRCLE('',#11520,0.15);
#4737=CIRCLE('',#11522,0.275);
#4738=CIRCLE('',#11525,0.15);
#4739=CIRCLE('',#11536,0.275);
#4740=CIRCLE('',#11537,0.15);
#4741=CIRCLE('',#11539,0.275);
#4742=CIRCLE('',#11542,0.15);
#4743=CIRCLE('',#11553,0.275);
#4744=CIRCLE('',#11554,0.15);
#4745=CIRCLE('',#11556,0.275);
#4746=CIRCLE('',#11559,0.15);
#4747=CIRCLE('',#11570,0.275);
#4748=CIRCLE('',#11571,0.15);
#4749=CIRCLE('',#11573,0.275);
#4750=CIRCLE('',#11576,0.15);
#4751=CIRCLE('',#11581,2.05);
#4752=CIRCLE('',#11583,2.05);
#4753=CIRCLE('',#11584,2.05);
#4754=CIRCLE('',#11585,2.05);
#4755=CIRCLE('',#11586,2.05);
#4756=CIRCLE('',#11588,2.05);
#4757=CIRCLE('',#11589,2.05);
#4758=CIRCLE('',#11590,2.05);
#4759=CIRCLE('',#11593,2.8);
#4760=CIRCLE('',#11595,2.35);
#4761=CIRCLE('',#11597,2.8);
#4762=CIRCLE('',#11599,2.8);
#4763=CIRCLE('',#11601,2.8);
#4764=CIRCLE('',#11604,2.8);
#4765=CIRCLE('',#11607,0.65);
#4766=CIRCLE('',#11608,0.65);
#4767=CIRCLE('',#11610,2.8);
#4768=CIRCLE('',#11611,2.8);
#4769=CIRCLE('',#11613,2.8);
#4770=CIRCLE('',#11622,0.65);
#4771=CIRCLE('',#11624,0.65);
#4772=CIRCLE('',#11632,1.8);
#4773=CIRCLE('',#11633,1.8);
#4774=CIRCLE('',#11635,2.19089023002066);
#4775=CIRCLE('',#11637,2.35);
#4776=CIRCLE('',#11638,2.19089023002066);
#4777=CIRCLE('',#11643,1.65);
#4778=CIRCLE('',#11644,1.65);
#4779=CIRCLE('',#11650,0.6);
#4780=CIRCLE('',#11652,1.75);
#4781=CIRCLE('',#11654,1.75);
#4782=CIRCLE('',#11656,0.6);
#4783=CIRCLE('',#11662,0.42);
#4784=CIRCLE('',#11663,0.42);
#4785=CIRCLE('',#11665,0.8);
#4786=CIRCLE('',#11666,0.8);
#4787=CIRCLE('',#11679,0.3933);
#4788=CIRCLE('',#11681,0.6);
#4789=CIRCLE('',#11683,0.65);
#4790=CIRCLE('',#11685,0.65);
#4791=CIRCLE('',#11687,0.62);
#4792=CIRCLE('',#11689,0.42);
#4793=CIRCLE('',#11691,0.3933);
#4794=CIRCLE('',#11703,0.24505);
#4795=CIRCLE('',#11705,0.375);
#4796=CIRCLE('',#11707,0.425);
#4797=CIRCLE('',#11709,0.425);
#4798=CIRCLE('',#11711,0.395);
#4799=CIRCLE('',#11713,0.27);
#4800=CIRCLE('',#11715,0.24505);
#4801=CIRCLE('',#11746,0.6);
#4802=CIRCLE('',#11750,0.6);
#4803=CIRCLE('',#11752,0.165);
#4804=CIRCLE('',#11753,0.165);
#4805=CIRCLE('',#11756,0.6);
#4806=CIRCLE('',#11757,0.6);
#4807=CIRCLE('',#11762,0.25);
#4808=CIRCLE('',#11763,0.25);
#4809=CIRCLE('',#11768,0.165);
#4810=CIRCLE('',#11770,0.165);
#4811=CIRCLE('',#11771,0.165);
#4812=CIRCLE('',#11774,0.25);
#4813=CIRCLE('',#11775,0.25);
#4814=CIRCLE('',#11777,0.6);
#4815=CIRCLE('',#11778,0.6);
#4816=CIRCLE('',#11783,0.21);
#4817=CIRCLE('',#11785,0.21);
#4818=CIRCLE('',#11786,0.21);
#4819=CIRCLE('',#11792,1.2);
#4820=CIRCLE('',#11793,0.6);
#4821=CIRCLE('',#11795,0.6);
#4822=CIRCLE('',#11797,2.8);
#4823=CIRCLE('',#11798,1.2);
#4824=CIRCLE('',#11800,2.8);
#4825=CIRCLE('',#11801,1.2);
#4826=CIRCLE('',#11804,1.2);
#4827=CIRCLE('',#11809,0.21);
#4828=CIRCLE('',#11811,0.21);
#4829=CIRCLE('',#11812,0.21);
#4830=CIRCLE('',#11815,0.605);
#4831=CIRCLE('',#11816,0.605);
#4832=CIRCLE('',#11818,1.1);
#4833=CIRCLE('',#11819,1.1);
#4834=CIRCLE('',#11824,0.21);
#4835=CIRCLE('',#11826,0.21);
#4836=CIRCLE('',#11827,0.21);
#4837=CIRCLE('',#11830,0.605);
#4838=CIRCLE('',#11831,0.605);
#4839=CIRCLE('',#11833,1.1);
#4840=CIRCLE('',#11834,1.1);
#4841=CIRCLE('',#11839,0.225);
#4842=CIRCLE('',#11840,0.225);
#4843=CIRCLE('',#11842,0.8);
#4844=CIRCLE('',#11843,0.8);
#4845=CIRCLE('',#11855,0.17);
#4846=CIRCLE('',#11857,0.1954);
#4847=CIRCLE('',#11859,0.1954);
#4848=CIRCLE('',#11861,0.125);
#4849=CIRCLE('',#11867,0.6);
#4850=CIRCLE('',#11868,0.6);
#4851=CIRCLE('',#11889,1.37);
#4852=CIRCLE('',#11891,1.37);
#4853=CIRCLE('',#11893,1.37);
#4854=CIRCLE('',#11895,1.37);
#4855=CIRCLE('',#11897,1.37);
#4856=CIRCLE('',#11899,1.37);
#4857=CIRCLE('',#11901,1.37);
#4858=CIRCLE('',#11903,1.37);
#4859=CIRCLE('',#11905,1.37);
#4860=CIRCLE('',#11906,1.37);
#4861=CIRCLE('',#11907,1.37);
#4862=CIRCLE('',#11908,1.37);
#4863=CIRCLE('',#11929,1.37);
#4864=CIRCLE('',#11931,1.37);
#4865=CIRCLE('',#11933,1.37);
#4866=CIRCLE('',#11935,1.37);
#4867=CIRCLE('',#11937,1.37);
#4868=CIRCLE('',#11939,1.37);
#4869=CIRCLE('',#11941,1.37);
#4870=CIRCLE('',#11943,1.37);
#4871=CIRCLE('',#11964,1.37);
#4872=CIRCLE('',#11966,1.37);
#4873=CIRCLE('',#11968,1.37);
#4874=CIRCLE('',#11970,1.37);
#4875=CIRCLE('',#11972,1.37);
#4876=CIRCLE('',#11974,1.37);
#4877=CIRCLE('',#11976,1.37);
#4878=CIRCLE('',#11978,1.37);
#4879=CIRCLE('',#11980,1.37);
#4880=CIRCLE('',#11985,0.6);
#4881=CIRCLE('',#11986,0.6);
#4882=CIRCLE('',#12007,1.37);
#4883=CIRCLE('',#12009,1.37);
#4884=CIRCLE('',#12011,1.37);
#4885=CIRCLE('',#12013,1.37);
#4886=CIRCLE('',#12015,1.37);
#4887=CIRCLE('',#12017,1.37);
#4888=CIRCLE('',#12019,1.37);
#4889=CIRCLE('',#12020,1.37);
#4890=CIRCLE('',#12021,1.37);
#4891=CIRCLE('',#12022,1.37);
#4892=CIRCLE('',#12024,1.37);
#4893=CIRCLE('',#12026,1.37);
#4894=CIRCLE('',#12047,1.37);
#4895=CIRCLE('',#12049,1.37);
#4896=CIRCLE('',#12051,1.37);
#4897=CIRCLE('',#12053,1.37);
#4898=CIRCLE('',#12055,1.37);
#4899=CIRCLE('',#12057,1.37);
#4900=CIRCLE('',#12059,1.37);
#4901=CIRCLE('',#12061,1.37);
#4902=CIRCLE('',#12082,1.37);
#4903=CIRCLE('',#12084,1.37);
#4904=CIRCLE('',#12086,1.37);
#4905=CIRCLE('',#12088,1.37);
#4906=CIRCLE('',#12090,1.37);
#4907=CIRCLE('',#12092,1.37);
#4908=CIRCLE('',#12094,1.37);
#4909=CIRCLE('',#12096,1.37);
#4910=CIRCLE('',#12098,1.37);
#4911=CIRCLE('',#12102,0.817);
#4912=CIRCLE('',#12103,0.817);
#4913=CIRCLE('',#12104,0.817);
#4914=CIRCLE('',#12105,0.817);
#4915=CIRCLE('',#12106,0.817);
#4916=CIRCLE('',#12107,0.817);
#4917=CIRCLE('',#12109,0.817);
#4918=CIRCLE('',#12111,0.817);
#4919=CIRCLE('',#12113,0.817);
#4920=CIRCLE('',#12115,0.817);
#4921=CIRCLE('',#12117,0.817);
#4922=CIRCLE('',#12119,0.817);
#4923=CIRCLE('',#12259,0.16);
#4924=CIRCLE('',#12260,0.2);
#4925=CIRCLE('',#12263,0.16);
#4926=CIRCLE('',#12264,0.2);
#4927=CIRCLE('',#12266,0.2);
#4928=CIRCLE('',#12271,0.16);
#4929=CIRCLE('',#12274,0.2);
#4930=CIRCLE('',#12275,0.16);
#4931=CIRCLE('',#12288,0.22);
#4932=CIRCLE('',#12290,0.24505);
#4933=CIRCLE('',#12292,0.24505);
#4934=CIRCLE('',#12294,0.175);
#4935=CIRCLE('',#12298,0.3);
#4936=CIRCLE('',#12300,0.35);
#4937=CIRCLE('',#12302,0.35);
#4938=CIRCLE('',#12304,0.32);
#4939=CIRCLE('',#12306,0.22);
#4940=CIRCLE('',#12308,0.1954);
#4941=CIRCLE('',#12310,0.1954);
#4942=CIRCLE('',#12312,0.16);
#4943=VERTEX_POINT('',#15431);
#4944=VERTEX_POINT('',#15433);
#4945=VERTEX_POINT('',#15437);
#4946=VERTEX_POINT('',#15439);
#4947=VERTEX_POINT('',#15443);
#4948=VERTEX_POINT('',#15445);
#4949=VERTEX_POINT('',#15449);
#4950=VERTEX_POINT('',#15451);
#4951=VERTEX_POINT('',#15455);
#4952=VERTEX_POINT('',#15457);
#4953=VERTEX_POINT('',#15461);
#4954=VERTEX_POINT('',#15463);
#4955=VERTEX_POINT('',#15467);
#4956=VERTEX_POINT('',#15468);
#4957=VERTEX_POINT('',#15470);
#4958=VERTEX_POINT('',#15472);
#4959=VERTEX_POINT('',#15476);
#4960=VERTEX_POINT('',#15478);
#4961=VERTEX_POINT('',#15482);
#4962=VERTEX_POINT('',#15484);
#4963=VERTEX_POINT('',#15494);
#4964=VERTEX_POINT('',#15495);
#4965=VERTEX_POINT('',#15497);
#4966=VERTEX_POINT('',#15499);
#4967=VERTEX_POINT('',#15503);
#4968=VERTEX_POINT('',#15505);
#4969=VERTEX_POINT('',#15509);
#4970=VERTEX_POINT('',#15511);
#4971=VERTEX_POINT('',#15521);
#4972=VERTEX_POINT('',#15522);
#4973=VERTEX_POINT('',#15524);
#4974=VERTEX_POINT('',#15526);
#4975=VERTEX_POINT('',#15530);
#4976=VERTEX_POINT('',#15532);
#4977=VERTEX_POINT('',#15536);
#4978=VERTEX_POINT('',#15538);
#4979=VERTEX_POINT('',#15548);
#4980=VERTEX_POINT('',#15550);
#4981=VERTEX_POINT('',#15554);
#4982=VERTEX_POINT('',#15556);
#4983=VERTEX_POINT('',#15563);
#4984=VERTEX_POINT('',#15565);
#4985=VERTEX_POINT('',#15569);
#4986=VERTEX_POINT('',#15571);
#4987=VERTEX_POINT('',#15578);
#4988=VERTEX_POINT('',#15580);
#4989=VERTEX_POINT('',#15584);
#4990=VERTEX_POINT('',#15586);
#4991=VERTEX_POINT('',#15593);
#4992=VERTEX_POINT('',#15595);
#4993=VERTEX_POINT('',#15599);
#4994=VERTEX_POINT('',#15601);
#4995=VERTEX_POINT('',#15608);
#4996=VERTEX_POINT('',#15610);
#4997=VERTEX_POINT('',#15614);
#4998=VERTEX_POINT('',#15616);
#4999=VERTEX_POINT('',#15620);
#5000=VERTEX_POINT('',#15622);
#5001=VERTEX_POINT('',#15626);
#5002=VERTEX_POINT('',#15628);
#5003=VERTEX_POINT('',#15632);
#5004=VERTEX_POINT('',#15634);
#5005=VERTEX_POINT('',#15638);
#5006=VERTEX_POINT('',#15640);
#5007=VERTEX_POINT('',#15644);
#5008=VERTEX_POINT('',#15646);
#5009=VERTEX_POINT('',#15650);
#5010=VERTEX_POINT('',#15651);
#5011=VERTEX_POINT('',#15653);
#5012=VERTEX_POINT('',#15655);
#5013=VERTEX_POINT('',#15659);
#5014=VERTEX_POINT('',#15661);
#5015=VERTEX_POINT('',#15665);
#5016=VERTEX_POINT('',#15666);
#5017=VERTEX_POINT('',#15668);
#5018=VERTEX_POINT('',#15670);
#5019=VERTEX_POINT('',#15674);
#5020=VERTEX_POINT('',#15679);
#5021=VERTEX_POINT('',#15689);
#5022=VERTEX_POINT('',#15691);
#5023=VERTEX_POINT('',#15696);
#5024=VERTEX_POINT('',#15698);
#5025=VERTEX_POINT('',#15703);
#5026=VERTEX_POINT('',#15705);
#5027=VERTEX_POINT('',#15710);
#5028=VERTEX_POINT('',#15712);
#5029=VERTEX_POINT('',#15717);
#5030=VERTEX_POINT('',#15719);
#5031=VERTEX_POINT('',#15723);
#5032=VERTEX_POINT('',#15726);
#5033=VERTEX_POINT('',#15730);
#5034=VERTEX_POINT('',#15731);
#5035=VERTEX_POINT('',#15733);
#5036=VERTEX_POINT('',#15735);
#5037=VERTEX_POINT('',#15739);
#5038=VERTEX_POINT('',#15741);
#5039=VERTEX_POINT('',#15745);
#5040=VERTEX_POINT('',#15747);
#5041=VERTEX_POINT('',#15757);
#5042=VERTEX_POINT('',#15758);
#5043=VERTEX_POINT('',#15760);
#5044=VERTEX_POINT('',#15762);
#5045=VERTEX_POINT('',#15766);
#5046=VERTEX_POINT('',#15768);
#5047=VERTEX_POINT('',#15772);
#5048=VERTEX_POINT('',#15774);
#5049=VERTEX_POINT('',#15778);
#5050=VERTEX_POINT('',#15780);
#5051=VERTEX_POINT('',#15784);
#5052=VERTEX_POINT('',#15786);
#5053=VERTEX_POINT('',#15794);
#5054=VERTEX_POINT('',#15796);
#5055=VERTEX_POINT('',#15799);
#5056=VERTEX_POINT('',#15804);
#5057=VERTEX_POINT('',#15810);
#5058=VERTEX_POINT('',#15811);
#5059=VERTEX_POINT('',#15813);
#5060=VERTEX_POINT('',#15815);
#5061=VERTEX_POINT('',#15819);
#5062=VERTEX_POINT('',#15821);
#5063=VERTEX_POINT('',#15825);
#5064=VERTEX_POINT('',#15827);
#5065=VERTEX_POINT('',#15831);
#5066=VERTEX_POINT('',#15833);
#5067=VERTEX_POINT('',#15837);
#5068=VERTEX_POINT('',#15839);
#5069=VERTEX_POINT('',#15847);
#5070=VERTEX_POINT('',#15849);
#5071=VERTEX_POINT('',#15852);
#5072=VERTEX_POINT('',#15857);
#5073=VERTEX_POINT('',#15863);
#5074=VERTEX_POINT('',#15864);
#5075=VERTEX_POINT('',#15866);
#5076=VERTEX_POINT('',#15868);
#5077=VERTEX_POINT('',#15872);
#5078=VERTEX_POINT('',#15874);
#5079=VERTEX_POINT('',#15878);
#5080=VERTEX_POINT('',#15880);
#5081=VERTEX_POINT('',#15884);
#5082=VERTEX_POINT('',#15886);
#5083=VERTEX_POINT('',#15890);
#5084=VERTEX_POINT('',#15892);
#5085=VERTEX_POINT('',#15900);
#5086=VERTEX_POINT('',#15902);
#5087=VERTEX_POINT('',#15905);
#5088=VERTEX_POINT('',#15910);
#5089=VERTEX_POINT('',#15916);
#5090=VERTEX_POINT('',#15917);
#5091=VERTEX_POINT('',#15919);
#5092=VERTEX_POINT('',#15921);
#5093=VERTEX_POINT('',#15925);
#5094=VERTEX_POINT('',#15927);
#5095=VERTEX_POINT('',#15931);
#5096=VERTEX_POINT('',#15933);
#5097=VERTEX_POINT('',#15937);
#5098=VERTEX_POINT('',#15939);
#5099=VERTEX_POINT('',#15943);
#5100=VERTEX_POINT('',#15945);
#5101=VERTEX_POINT('',#15953);
#5102=VERTEX_POINT('',#15955);
#5103=VERTEX_POINT('',#15958);
#5104=VERTEX_POINT('',#15963);
#5105=VERTEX_POINT('',#15970);
#5106=VERTEX_POINT('',#15971);
#5107=VERTEX_POINT('',#15975);
#5108=VERTEX_POINT('',#15976);
#5109=VERTEX_POINT('',#15978);
#5110=VERTEX_POINT('',#15980);
#5111=VERTEX_POINT('',#15982);
#5112=VERTEX_POINT('',#15984);
#5113=VERTEX_POINT('',#15989);
#5114=VERTEX_POINT('',#15991);
#5115=VERTEX_POINT('',#15993);
#5116=VERTEX_POINT('',#15996);
#5117=VERTEX_POINT('',#16002);
#5118=VERTEX_POINT('',#16004);
#5119=VERTEX_POINT('',#16008);
#5120=VERTEX_POINT('',#16009);
#5121=VERTEX_POINT('',#16012);
#5122=VERTEX_POINT('',#16013);
#5123=VERTEX_POINT('',#16015);
#5124=VERTEX_POINT('',#16019);
#5125=VERTEX_POINT('',#16020);
#5126=VERTEX_POINT('',#16022);
#5127=VERTEX_POINT('',#16026);
#5128=VERTEX_POINT('',#16027);
#5129=VERTEX_POINT('',#16029);
#5130=VERTEX_POINT('',#16036);
#5131=VERTEX_POINT('',#16037);
#5132=VERTEX_POINT('',#16039);
#5133=VERTEX_POINT('',#16046);
#5134=VERTEX_POINT('',#16047);
#5135=VERTEX_POINT('',#16049);
#5136=VERTEX_POINT('',#16051);
#5137=VERTEX_POINT('',#16055);
#5138=VERTEX_POINT('',#16058);
#5139=VERTEX_POINT('',#16062);
#5140=VERTEX_POINT('',#16064);
#5141=VERTEX_POINT('',#16067);
#5142=VERTEX_POINT('',#16068);
#5143=VERTEX_POINT('',#16070);
#5144=VERTEX_POINT('',#16072);
#5145=VERTEX_POINT('',#16079);
#5146=VERTEX_POINT('',#16081);
#5147=VERTEX_POINT('',#16083);
#5148=VERTEX_POINT('',#16085);
#5149=VERTEX_POINT('',#16089);
#5150=VERTEX_POINT('',#16093);
#5151=VERTEX_POINT('',#16095);
#5152=VERTEX_POINT('',#16100);
#5153=VERTEX_POINT('',#16107);
#5154=VERTEX_POINT('',#16111);
#5155=VERTEX_POINT('',#16115);
#5156=VERTEX_POINT('',#16116);
#5157=VERTEX_POINT('',#16121);
#5158=VERTEX_POINT('',#16125);
#5159=VERTEX_POINT('',#16133);
#5160=VERTEX_POINT('',#16135);
#5161=VERTEX_POINT('',#16139);
#5162=VERTEX_POINT('',#16142);
#5163=VERTEX_POINT('',#16143);
#5164=VERTEX_POINT('',#16145);
#5165=VERTEX_POINT('',#16149);
#5166=VERTEX_POINT('',#16150);
#5167=VERTEX_POINT('',#16161);
#5168=VERTEX_POINT('',#16190);
#5169=VERTEX_POINT('',#16227);
#5170=VERTEX_POINT('',#16262);
#5171=VERTEX_POINT('',#16264);
#5172=VERTEX_POINT('',#16275);
#5173=VERTEX_POINT('',#16305);
#5174=VERTEX_POINT('',#16307);
#5175=VERTEX_POINT('',#16310);
#5176=VERTEX_POINT('',#16311);
#5177=VERTEX_POINT('',#16330);
#5178=VERTEX_POINT('',#16351);
#5179=VERTEX_POINT('',#16352);
#5180=VERTEX_POINT('',#16371);
#5181=VERTEX_POINT('',#16392);
#5182=VERTEX_POINT('',#16393);
#5183=VERTEX_POINT('',#16412);
#5184=VERTEX_POINT('',#16433);
#5185=VERTEX_POINT('',#16434);
#5186=VERTEX_POINT('',#16453);
#5187=VERTEX_POINT('',#16475);
#5188=VERTEX_POINT('',#16512);
#5189=VERTEX_POINT('',#16549);
#5190=VERTEX_POINT('',#16586);
#5191=VERTEX_POINT('',#16623);
#5192=VERTEX_POINT('',#16626);
#5193=VERTEX_POINT('',#16629);
#5194=VERTEX_POINT('',#16633);
#5195=VERTEX_POINT('',#16641);
#5196=VERTEX_POINT('',#16643);
#5197=VERTEX_POINT('',#16647);
#5198=VERTEX_POINT('',#16649);
#5199=VERTEX_POINT('',#16656);
#5200=VERTEX_POINT('',#16657);
#5201=VERTEX_POINT('',#16659);
#5202=VERTEX_POINT('',#16661);
#5203=VERTEX_POINT('',#16665);
#5204=VERTEX_POINT('',#16667);
#5205=VERTEX_POINT('',#16671);
#5206=VERTEX_POINT('',#16673);
#5207=VERTEX_POINT('',#16677);
#5208=VERTEX_POINT('',#16679);
#5209=VERTEX_POINT('',#16683);
#5210=VERTEX_POINT('',#16685);
#5211=VERTEX_POINT('',#16694);
#5212=VERTEX_POINT('',#16697);
#5213=VERTEX_POINT('',#16700);
#5214=VERTEX_POINT('',#16704);
#5215=VERTEX_POINT('',#16708);
#5216=VERTEX_POINT('',#16712);
#5217=VERTEX_POINT('',#16715);
#5218=VERTEX_POINT('',#16722);
#5219=VERTEX_POINT('',#16723);
#5220=VERTEX_POINT('',#16725);
#5221=VERTEX_POINT('',#16727);
#5222=VERTEX_POINT('',#16731);
#5223=VERTEX_POINT('',#16733);
#5224=VERTEX_POINT('',#16737);
#5225=VERTEX_POINT('',#16739);
#5226=VERTEX_POINT('',#16743);
#5227=VERTEX_POINT('',#16745);
#5228=VERTEX_POINT('',#16749);
#5229=VERTEX_POINT('',#16751);
#5230=VERTEX_POINT('',#16760);
#5231=VERTEX_POINT('',#16763);
#5232=VERTEX_POINT('',#16766);
#5233=VERTEX_POINT('',#16770);
#5234=VERTEX_POINT('',#16774);
#5235=VERTEX_POINT('',#16778);
#5236=VERTEX_POINT('',#16781);
#5237=VERTEX_POINT('',#16814);
#5238=VERTEX_POINT('',#16815);
#5239=VERTEX_POINT('',#16817);
#5240=VERTEX_POINT('',#16819);
#5241=VERTEX_POINT('',#16823);
#5242=VERTEX_POINT('',#16825);
#5243=VERTEX_POINT('',#16829);
#5244=VERTEX_POINT('',#16831);
#5245=VERTEX_POINT('',#16839);
#5246=VERTEX_POINT('',#16841);
#5247=VERTEX_POINT('',#16846);
#5248=VERTEX_POINT('',#16848);
#5249=VERTEX_POINT('',#16855);
#5250=VERTEX_POINT('',#16857);
#5251=VERTEX_POINT('',#16864);
#5252=VERTEX_POINT('',#16865);
#5253=VERTEX_POINT('',#16869);
#5254=VERTEX_POINT('',#16880);
#5255=VERTEX_POINT('',#16882);
#5256=VERTEX_POINT('',#16884);
#5257=VERTEX_POINT('',#16921);
#5258=VERTEX_POINT('',#16936);
#5259=VERTEX_POINT('',#16938);
#5260=VERTEX_POINT('',#16942);
#5261=VERTEX_POINT('',#16944);
#5262=VERTEX_POINT('',#16951);
#5263=VERTEX_POINT('',#16952);
#5264=VERTEX_POINT('',#16956);
#5265=VERTEX_POINT('',#16967);
#5266=VERTEX_POINT('',#16969);
#5267=VERTEX_POINT('',#16971);
#5268=VERTEX_POINT('',#17008);
#5269=VERTEX_POINT('',#17023);
#5270=VERTEX_POINT('',#17024);
#5271=VERTEX_POINT('',#17026);
#5272=VERTEX_POINT('',#17028);
#5273=VERTEX_POINT('',#17032);
#5274=VERTEX_POINT('',#17034);
#5275=VERTEX_POINT('',#17038);
#5276=VERTEX_POINT('',#17040);
#5277=VERTEX_POINT('',#17044);
#5278=VERTEX_POINT('',#17050);
#5279=VERTEX_POINT('',#17052);
#5280=VERTEX_POINT('',#17055);
#5281=VERTEX_POINT('',#17057);
#5282=VERTEX_POINT('',#17062);
#5283=VERTEX_POINT('',#17070);
#5284=VERTEX_POINT('',#17071);
#5285=VERTEX_POINT('',#17075);
#5286=VERTEX_POINT('',#17086);
#5287=VERTEX_POINT('',#17088);
#5288=VERTEX_POINT('',#17090);
#5289=VERTEX_POINT('',#17127);
#5290=VERTEX_POINT('',#17142);
#5291=VERTEX_POINT('',#17144);
#5292=VERTEX_POINT('',#17148);
#5293=VERTEX_POINT('',#17150);
#5294=VERTEX_POINT('',#17157);
#5295=VERTEX_POINT('',#17158);
#5296=VERTEX_POINT('',#17162);
#5297=VERTEX_POINT('',#17173);
#5298=VERTEX_POINT('',#17175);
#5299=VERTEX_POINT('',#17177);
#5300=VERTEX_POINT('',#17214);
#5301=VERTEX_POINT('',#17229);
#5302=VERTEX_POINT('',#17231);
#5303=VERTEX_POINT('',#17235);
#5304=VERTEX_POINT('',#17237);
#5305=VERTEX_POINT('',#17244);
#5306=VERTEX_POINT('',#17246);
#5307=VERTEX_POINT('',#17250);
#5308=VERTEX_POINT('',#17252);
#5309=VERTEX_POINT('',#17259);
#5310=VERTEX_POINT('',#17260);
#5311=VERTEX_POINT('',#17262);
#5312=VERTEX_POINT('',#17264);
#5313=VERTEX_POINT('',#17268);
#5314=VERTEX_POINT('',#17270);
#5315=VERTEX_POINT('',#17274);
#5316=VERTEX_POINT('',#17276);
#5317=VERTEX_POINT('',#17280);
#5318=VERTEX_POINT('',#17282);
#5319=VERTEX_POINT('',#17286);
#5320=VERTEX_POINT('',#17288);
#5321=VERTEX_POINT('',#17296);
#5322=VERTEX_POINT('',#17299);
#5323=VERTEX_POINT('',#17303);
#5324=VERTEX_POINT('',#17307);
#5325=VERTEX_POINT('',#17314);
#5326=VERTEX_POINT('',#17315);
#5327=VERTEX_POINT('',#17352);
#5328=VERTEX_POINT('',#17389);
#5329=VERTEX_POINT('',#17391);
#5330=VERTEX_POINT('',#17395);
#5331=VERTEX_POINT('',#17396);
#5332=VERTEX_POINT('',#17398);
#5333=VERTEX_POINT('',#17400);
#5334=VERTEX_POINT('',#17404);
#5335=VERTEX_POINT('',#17406);
#5336=VERTEX_POINT('',#17410);
#5337=VERTEX_POINT('',#17412);
#5338=VERTEX_POINT('',#17416);
#5339=VERTEX_POINT('',#17418);
#5340=VERTEX_POINT('',#17422);
#5341=VERTEX_POINT('',#17424);
#5342=VERTEX_POINT('',#17428);
#5343=VERTEX_POINT('',#17430);
#5344=VERTEX_POINT('',#17434);
#5345=VERTEX_POINT('',#17436);
#5346=VERTEX_POINT('',#17440);
#5347=VERTEX_POINT('',#17442);
#5348=VERTEX_POINT('',#17446);
#5349=VERTEX_POINT('',#17448);
#5350=VERTEX_POINT('',#17452);
#5351=VERTEX_POINT('',#17454);
#5352=VERTEX_POINT('',#17458);
#5353=VERTEX_POINT('',#17460);
#5354=VERTEX_POINT('',#17464);
#5355=VERTEX_POINT('',#17466);
#5356=VERTEX_POINT('',#17470);
#5357=VERTEX_POINT('',#17472);
#5358=VERTEX_POINT('',#17476);
#5359=VERTEX_POINT('',#17478);
#5360=VERTEX_POINT('',#17482);
#5361=VERTEX_POINT('',#17484);
#5362=VERTEX_POINT('',#17488);
#5363=VERTEX_POINT('',#17490);
#5364=VERTEX_POINT('',#17494);
#5365=VERTEX_POINT('',#17496);
#5366=VERTEX_POINT('',#17520);
#5367=VERTEX_POINT('',#17522);
#5368=VERTEX_POINT('',#17524);
#5369=VERTEX_POINT('',#17526);
#5370=VERTEX_POINT('',#17528);
#5371=VERTEX_POINT('',#17530);
#5372=VERTEX_POINT('',#17532);
#5373=VERTEX_POINT('',#17534);
#5374=VERTEX_POINT('',#17536);
#5375=VERTEX_POINT('',#17538);
#5376=VERTEX_POINT('',#17540);
#5377=VERTEX_POINT('',#17542);
#5378=VERTEX_POINT('',#17544);
#5379=VERTEX_POINT('',#17546);
#5380=VERTEX_POINT('',#17548);
#5381=VERTEX_POINT('',#17550);
#5382=VERTEX_POINT('',#17552);
#5383=VERTEX_POINT('',#17554);
#5384=VERTEX_POINT('',#17556);
#5385=VERTEX_POINT('',#17558);
#5386=VERTEX_POINT('',#17560);
#5387=VERTEX_POINT('',#17562);
#5388=VERTEX_POINT('',#17564);
#5389=VERTEX_POINT('',#17568);
#5390=VERTEX_POINT('',#17569);
#5391=VERTEX_POINT('',#17572);
#5392=VERTEX_POINT('',#17576);
#5393=VERTEX_POINT('',#17578);
#5394=VERTEX_POINT('',#17582);
#5395=VERTEX_POINT('',#17584);
#5396=VERTEX_POINT('',#17588);
#5397=VERTEX_POINT('',#17590);
#5398=VERTEX_POINT('',#17594);
#5399=VERTEX_POINT('',#17596);
#5400=VERTEX_POINT('',#17600);
#5401=VERTEX_POINT('',#17602);
#5402=VERTEX_POINT('',#17606);
#5403=VERTEX_POINT('',#17608);
#5404=VERTEX_POINT('',#17612);
#5405=VERTEX_POINT('',#17617);
#5406=VERTEX_POINT('',#17621);
#5407=VERTEX_POINT('',#17625);
#5408=VERTEX_POINT('',#17629);
#5409=VERTEX_POINT('',#17633);
#5410=VERTEX_POINT('',#17637);
#5411=VERTEX_POINT('',#17641);
#5412=VERTEX_POINT('',#17645);
#5413=VERTEX_POINT('',#17649);
#5414=VERTEX_POINT('',#17672);
#5415=VERTEX_POINT('',#17673);
#5416=VERTEX_POINT('',#17676);
#5417=VERTEX_POINT('',#17680);
#5418=VERTEX_POINT('',#17682);
#5419=VERTEX_POINT('',#17686);
#5420=VERTEX_POINT('',#17688);
#5421=VERTEX_POINT('',#17692);
#5422=VERTEX_POINT('',#17694);
#5423=VERTEX_POINT('',#17698);
#5424=VERTEX_POINT('',#17700);
#5425=VERTEX_POINT('',#17704);
#5426=VERTEX_POINT('',#17706);
#5427=VERTEX_POINT('',#17710);
#5428=VERTEX_POINT('',#17712);
#5429=VERTEX_POINT('',#17716);
#5430=VERTEX_POINT('',#17721);
#5431=VERTEX_POINT('',#17725);
#5432=VERTEX_POINT('',#17729);
#5433=VERTEX_POINT('',#17733);
#5434=VERTEX_POINT('',#17737);
#5435=VERTEX_POINT('',#17741);
#5436=VERTEX_POINT('',#17745);
#5437=VERTEX_POINT('',#17749);
#5438=VERTEX_POINT('',#17753);
#5439=VERTEX_POINT('',#17776);
#5440=VERTEX_POINT('',#17782);
#5441=VERTEX_POINT('',#17783);
#5442=VERTEX_POINT('',#17820);
#5443=VERTEX_POINT('',#17822);
#5444=VERTEX_POINT('',#17860);
#5445=VERTEX_POINT('',#17862);
#5446=VERTEX_POINT('',#17866);
#5447=VERTEX_POINT('',#17867);
#5448=VERTEX_POINT('',#17869);
#5449=VERTEX_POINT('',#17871);
#5450=VERTEX_POINT('',#17875);
#5451=VERTEX_POINT('',#17877);
#5452=VERTEX_POINT('',#17881);
#5453=VERTEX_POINT('',#17883);
#5454=VERTEX_POINT('',#17887);
#5455=VERTEX_POINT('',#17889);
#5456=VERTEX_POINT('',#17893);
#5457=VERTEX_POINT('',#17895);
#5458=VERTEX_POINT('',#17899);
#5459=VERTEX_POINT('',#17901);
#5460=VERTEX_POINT('',#17905);
#5461=VERTEX_POINT('',#17907);
#5462=VERTEX_POINT('',#17911);
#5463=VERTEX_POINT('',#17913);
#5464=VERTEX_POINT('',#17917);
#5465=VERTEX_POINT('',#17919);
#5466=VERTEX_POINT('',#17923);
#5467=VERTEX_POINT('',#17925);
#5468=VERTEX_POINT('',#17929);
#5469=VERTEX_POINT('',#17931);
#5470=VERTEX_POINT('',#17935);
#5471=VERTEX_POINT('',#17937);
#5472=VERTEX_POINT('',#17941);
#5473=VERTEX_POINT('',#17943);
#5474=VERTEX_POINT('',#17947);
#5475=VERTEX_POINT('',#17949);
#5476=VERTEX_POINT('',#17953);
#5477=VERTEX_POINT('',#17955);
#5478=VERTEX_POINT('',#17959);
#5479=VERTEX_POINT('',#17961);
#5480=VERTEX_POINT('',#17965);
#5481=VERTEX_POINT('',#17967);
#5482=VERTEX_POINT('',#17987);
#5483=VERTEX_POINT('',#17989);
#5484=VERTEX_POINT('',#17991);
#5485=VERTEX_POINT('',#17993);
#5486=VERTEX_POINT('',#17995);
#5487=VERTEX_POINT('',#17997);
#5488=VERTEX_POINT('',#17999);
#5489=VERTEX_POINT('',#18001);
#5490=VERTEX_POINT('',#18003);
#5491=VERTEX_POINT('',#18005);
#5492=VERTEX_POINT('',#18007);
#5493=VERTEX_POINT('',#18009);
#5494=VERTEX_POINT('',#18011);
#5495=VERTEX_POINT('',#18013);
#5496=VERTEX_POINT('',#18015);
#5497=VERTEX_POINT('',#18017);
#5498=VERTEX_POINT('',#18019);
#5499=VERTEX_POINT('',#18021);
#5500=VERTEX_POINT('',#18023);
#5501=VERTEX_POINT('',#18025);
#5502=VERTEX_POINT('',#18027);
#5503=VERTEX_POINT('',#18029);
#5504=VERTEX_POINT('',#18031);
#5505=VERTEX_POINT('',#18039);
#5506=VERTEX_POINT('',#18040);
#5507=VERTEX_POINT('',#18045);
#5508=VERTEX_POINT('',#18049);
#5509=VERTEX_POINT('',#18053);
#5510=VERTEX_POINT('',#18057);
#5511=VERTEX_POINT('',#18061);
#5512=VERTEX_POINT('',#18065);
#5513=VERTEX_POINT('',#18069);
#5514=VERTEX_POINT('',#18073);
#5515=VERTEX_POINT('',#18077);
#5516=VERTEX_POINT('',#18079);
#5517=VERTEX_POINT('',#18083);
#5518=VERTEX_POINT('',#18085);
#5519=VERTEX_POINT('',#18089);
#5520=VERTEX_POINT('',#18091);
#5521=VERTEX_POINT('',#18095);
#5522=VERTEX_POINT('',#18097);
#5523=VERTEX_POINT('',#18101);
#5524=VERTEX_POINT('',#18103);
#5525=VERTEX_POINT('',#18107);
#5526=VERTEX_POINT('',#18109);
#5527=VERTEX_POINT('',#18113);
#5528=VERTEX_POINT('',#18115);
#5529=VERTEX_POINT('',#18119);
#5530=VERTEX_POINT('',#18143);
#5531=VERTEX_POINT('',#18144);
#5532=VERTEX_POINT('',#18149);
#5533=VERTEX_POINT('',#18153);
#5534=VERTEX_POINT('',#18157);
#5535=VERTEX_POINT('',#18161);
#5536=VERTEX_POINT('',#18165);
#5537=VERTEX_POINT('',#18169);
#5538=VERTEX_POINT('',#18173);
#5539=VERTEX_POINT('',#18177);
#5540=VERTEX_POINT('',#18181);
#5541=VERTEX_POINT('',#18183);
#5542=VERTEX_POINT('',#18187);
#5543=VERTEX_POINT('',#18189);
#5544=VERTEX_POINT('',#18193);
#5545=VERTEX_POINT('',#18195);
#5546=VERTEX_POINT('',#18199);
#5547=VERTEX_POINT('',#18201);
#5548=VERTEX_POINT('',#18205);
#5549=VERTEX_POINT('',#18207);
#5550=VERTEX_POINT('',#18211);
#5551=VERTEX_POINT('',#18213);
#5552=VERTEX_POINT('',#18217);
#5553=VERTEX_POINT('',#18219);
#5554=VERTEX_POINT('',#18223);
#5555=VERTEX_POINT('',#18247);
#5556=VERTEX_POINT('',#18253);
#5557=VERTEX_POINT('',#18254);
#5558=VERTEX_POINT('',#18256);
#5559=VERTEX_POINT('',#18258);
#5560=VERTEX_POINT('',#18260);
#5561=VERTEX_POINT('',#18262);
#5562=VERTEX_POINT('',#18264);
#5563=VERTEX_POINT('',#18266);
#5564=VERTEX_POINT('',#18268);
#5565=VERTEX_POINT('',#18270);
#5566=VERTEX_POINT('',#18272);
#5567=VERTEX_POINT('',#18274);
#5568=VERTEX_POINT('',#18276);
#5569=VERTEX_POINT('',#18278);
#5570=VERTEX_POINT('',#18280);
#5571=VERTEX_POINT('',#18282);
#5572=VERTEX_POINT('',#18284);
#5573=VERTEX_POINT('',#18286);
#5574=VERTEX_POINT('',#18288);
#5575=VERTEX_POINT('',#18290);
#5576=VERTEX_POINT('',#18292);
#5577=VERTEX_POINT('',#18294);
#5578=VERTEX_POINT('',#18296);
#5579=VERTEX_POINT('',#18298);
#5580=VERTEX_POINT('',#18300);
#5581=VERTEX_POINT('',#18302);
#5582=VERTEX_POINT('',#18304);
#5583=VERTEX_POINT('',#18306);
#5584=VERTEX_POINT('',#18308);
#5585=VERTEX_POINT('',#18310);
#5586=VERTEX_POINT('',#18312);
#5587=VERTEX_POINT('',#18314);
#5588=VERTEX_POINT('',#18316);
#5589=VERTEX_POINT('',#18318);
#5590=VERTEX_POINT('',#18320);
#5591=VERTEX_POINT('',#18322);
#5592=VERTEX_POINT('',#18324);
#5593=VERTEX_POINT('',#18326);
#5594=VERTEX_POINT('',#18328);
#5595=VERTEX_POINT('',#18330);
#5596=VERTEX_POINT('',#18332);
#5597=VERTEX_POINT('',#18334);
#5598=VERTEX_POINT('',#18336);
#5599=VERTEX_POINT('',#18338);
#5600=VERTEX_POINT('',#18340);
#5601=VERTEX_POINT('',#18342);
#5602=VERTEX_POINT('',#18344);
#5603=VERTEX_POINT('',#18346);
#5604=VERTEX_POINT('',#18348);
#5605=VERTEX_POINT('',#18350);
#5606=VERTEX_POINT('',#18352);
#5607=VERTEX_POINT('',#18354);
#5608=VERTEX_POINT('',#18356);
#5609=VERTEX_POINT('',#18358);
#5610=VERTEX_POINT('',#18362);
#5611=VERTEX_POINT('',#18364);
#5612=VERTEX_POINT('',#18368);
#5613=VERTEX_POINT('',#18370);
#5614=VERTEX_POINT('',#18374);
#5615=VERTEX_POINT('',#18376);
#5616=VERTEX_POINT('',#18380);
#5617=VERTEX_POINT('',#18382);
#5618=VERTEX_POINT('',#18386);
#5619=VERTEX_POINT('',#18388);
#5620=VERTEX_POINT('',#18392);
#5621=VERTEX_POINT('',#18394);
#5622=VERTEX_POINT('',#18398);
#5623=VERTEX_POINT('',#18400);
#5624=VERTEX_POINT('',#18402);
#5625=VERTEX_POINT('',#18404);
#5626=VERTEX_POINT('',#18406);
#5627=VERTEX_POINT('',#18408);
#5628=VERTEX_POINT('',#18410);
#5629=VERTEX_POINT('',#18412);
#5630=VERTEX_POINT('',#18415);
#5631=VERTEX_POINT('',#18417);
#5632=VERTEX_POINT('',#18419);
#5633=VERTEX_POINT('',#18421);
#5634=VERTEX_POINT('',#18423);
#5635=VERTEX_POINT('',#18425);
#5636=VERTEX_POINT('',#18427);
#5637=VERTEX_POINT('',#18430);
#5638=VERTEX_POINT('',#18432);
#5639=VERTEX_POINT('',#18434);
#5640=VERTEX_POINT('',#18436);
#5641=VERTEX_POINT('',#18438);
#5642=VERTEX_POINT('',#18440);
#5643=VERTEX_POINT('',#18442);
#5644=VERTEX_POINT('',#18445);
#5645=VERTEX_POINT('',#18447);
#5646=VERTEX_POINT('',#18449);
#5647=VERTEX_POINT('',#18451);
#5648=VERTEX_POINT('',#18453);
#5649=VERTEX_POINT('',#18455);
#5650=VERTEX_POINT('',#18457);
#5651=VERTEX_POINT('',#18460);
#5652=VERTEX_POINT('',#18462);
#5653=VERTEX_POINT('',#18464);
#5654=VERTEX_POINT('',#18466);
#5655=VERTEX_POINT('',#18468);
#5656=VERTEX_POINT('',#18470);
#5657=VERTEX_POINT('',#18472);
#5658=VERTEX_POINT('',#18475);
#5659=VERTEX_POINT('',#18477);
#5660=VERTEX_POINT('',#18479);
#5661=VERTEX_POINT('',#18481);
#5662=VERTEX_POINT('',#18483);
#5663=VERTEX_POINT('',#18485);
#5664=VERTEX_POINT('',#18489);
#5665=VERTEX_POINT('',#18491);
#5666=VERTEX_POINT('',#18493);
#5667=VERTEX_POINT('',#18495);
#5668=VERTEX_POINT('',#18499);
#5669=VERTEX_POINT('',#18503);
#5670=VERTEX_POINT('',#18507);
#5671=VERTEX_POINT('',#18511);
#5672=VERTEX_POINT('',#18515);
#5673=VERTEX_POINT('',#18519);
#5674=VERTEX_POINT('',#18523);
#5675=VERTEX_POINT('',#18527);
#5676=VERTEX_POINT('',#18528);
#5677=VERTEX_POINT('',#18530);
#5678=VERTEX_POINT('',#18532);
#5679=VERTEX_POINT('',#18534);
#5680=VERTEX_POINT('',#18536);
#5681=VERTEX_POINT('',#18539);
#5682=VERTEX_POINT('',#18541);
#5683=VERTEX_POINT('',#18543);
#5684=VERTEX_POINT('',#18545);
#5685=VERTEX_POINT('',#18547);
#5686=VERTEX_POINT('',#18561);
#5687=VERTEX_POINT('',#18565);
#5688=VERTEX_POINT('',#18569);
#5689=VERTEX_POINT('',#18573);
#5690=VERTEX_POINT('',#18577);
#5691=VERTEX_POINT('',#18581);
#5692=VERTEX_POINT('',#18588);
#5693=VERTEX_POINT('',#18590);
#5694=VERTEX_POINT('',#18592);
#5695=VERTEX_POINT('',#18594);
#5696=VERTEX_POINT('',#18598);
#5697=VERTEX_POINT('',#18602);
#5698=VERTEX_POINT('',#18606);
#5699=VERTEX_POINT('',#18610);
#5700=VERTEX_POINT('',#18614);
#5701=VERTEX_POINT('',#18618);
#5702=VERTEX_POINT('',#18622);
#5703=VERTEX_POINT('',#18626);
#5704=VERTEX_POINT('',#18627);
#5705=VERTEX_POINT('',#18629);
#5706=VERTEX_POINT('',#18631);
#5707=VERTEX_POINT('',#18633);
#5708=VERTEX_POINT('',#18635);
#5709=VERTEX_POINT('',#18638);
#5710=VERTEX_POINT('',#18640);
#5711=VERTEX_POINT('',#18642);
#5712=VERTEX_POINT('',#18644);
#5713=VERTEX_POINT('',#18646);
#5714=VERTEX_POINT('',#18660);
#5715=VERTEX_POINT('',#18664);
#5716=VERTEX_POINT('',#18668);
#5717=VERTEX_POINT('',#18672);
#5718=VERTEX_POINT('',#18676);
#5719=VERTEX_POINT('',#18680);
#5720=VERTEX_POINT('',#18687);
#5721=VERTEX_POINT('',#18689);
#5722=VERTEX_POINT('',#18691);
#5723=VERTEX_POINT('',#18693);
#5724=VERTEX_POINT('',#18697);
#5725=VERTEX_POINT('',#18701);
#5726=VERTEX_POINT('',#18705);
#5727=VERTEX_POINT('',#18709);
#5728=VERTEX_POINT('',#18713);
#5729=VERTEX_POINT('',#18717);
#5730=VERTEX_POINT('',#18721);
#5731=VERTEX_POINT('',#18725);
#5732=VERTEX_POINT('',#18726);
#5733=VERTEX_POINT('',#18728);
#5734=VERTEX_POINT('',#18730);
#5735=VERTEX_POINT('',#18732);
#5736=VERTEX_POINT('',#18734);
#5737=VERTEX_POINT('',#18737);
#5738=VERTEX_POINT('',#18739);
#5739=VERTEX_POINT('',#18741);
#5740=VERTEX_POINT('',#18743);
#5741=VERTEX_POINT('',#18745);
#5742=VERTEX_POINT('',#18759);
#5743=VERTEX_POINT('',#18763);
#5744=VERTEX_POINT('',#18767);
#5745=VERTEX_POINT('',#18771);
#5746=VERTEX_POINT('',#18775);
#5747=VERTEX_POINT('',#18779);
#5748=VERTEX_POINT('',#18786);
#5749=VERTEX_POINT('',#18788);
#5750=VERTEX_POINT('',#18790);
#5751=VERTEX_POINT('',#18792);
#5752=VERTEX_POINT('',#18796);
#5753=VERTEX_POINT('',#18800);
#5754=VERTEX_POINT('',#18804);
#5755=VERTEX_POINT('',#18808);
#5756=VERTEX_POINT('',#18812);
#5757=VERTEX_POINT('',#18816);
#5758=VERTEX_POINT('',#18820);
#5759=VERTEX_POINT('',#18824);
#5760=VERTEX_POINT('',#18825);
#5761=VERTEX_POINT('',#18827);
#5762=VERTEX_POINT('',#18829);
#5763=VERTEX_POINT('',#18831);
#5764=VERTEX_POINT('',#18833);
#5765=VERTEX_POINT('',#18836);
#5766=VERTEX_POINT('',#18838);
#5767=VERTEX_POINT('',#18840);
#5768=VERTEX_POINT('',#18842);
#5769=VERTEX_POINT('',#18844);
#5770=VERTEX_POINT('',#18858);
#5771=VERTEX_POINT('',#18862);
#5772=VERTEX_POINT('',#18866);
#5773=VERTEX_POINT('',#18870);
#5774=VERTEX_POINT('',#18874);
#5775=VERTEX_POINT('',#18878);
#5776=VERTEX_POINT('',#18885);
#5777=VERTEX_POINT('',#18887);
#5778=VERTEX_POINT('',#18889);
#5779=VERTEX_POINT('',#18891);
#5780=VERTEX_POINT('',#18895);
#5781=VERTEX_POINT('',#18899);
#5782=VERTEX_POINT('',#18903);
#5783=VERTEX_POINT('',#18907);
#5784=VERTEX_POINT('',#18911);
#5785=VERTEX_POINT('',#18915);
#5786=VERTEX_POINT('',#18919);
#5787=VERTEX_POINT('',#18923);
#5788=VERTEX_POINT('',#18924);
#5789=VERTEX_POINT('',#18926);
#5790=VERTEX_POINT('',#18928);
#5791=VERTEX_POINT('',#18930);
#5792=VERTEX_POINT('',#18932);
#5793=VERTEX_POINT('',#18935);
#5794=VERTEX_POINT('',#18937);
#5795=VERTEX_POINT('',#18939);
#5796=VERTEX_POINT('',#18941);
#5797=VERTEX_POINT('',#18943);
#5798=VERTEX_POINT('',#18957);
#5799=VERTEX_POINT('',#18961);
#5800=VERTEX_POINT('',#18965);
#5801=VERTEX_POINT('',#18969);
#5802=VERTEX_POINT('',#18973);
#5803=VERTEX_POINT('',#18977);
#5804=VERTEX_POINT('',#18984);
#5805=VERTEX_POINT('',#18986);
#5806=VERTEX_POINT('',#18988);
#5807=VERTEX_POINT('',#18990);
#5808=VERTEX_POINT('',#18994);
#5809=VERTEX_POINT('',#18998);
#5810=VERTEX_POINT('',#19002);
#5811=VERTEX_POINT('',#19006);
#5812=VERTEX_POINT('',#19010);
#5813=VERTEX_POINT('',#19014);
#5814=VERTEX_POINT('',#19018);
#5815=VERTEX_POINT('',#19022);
#5816=VERTEX_POINT('',#19023);
#5817=VERTEX_POINT('',#19025);
#5818=VERTEX_POINT('',#19027);
#5819=VERTEX_POINT('',#19029);
#5820=VERTEX_POINT('',#19031);
#5821=VERTEX_POINT('',#19034);
#5822=VERTEX_POINT('',#19036);
#5823=VERTEX_POINT('',#19038);
#5824=VERTEX_POINT('',#19040);
#5825=VERTEX_POINT('',#19042);
#5826=VERTEX_POINT('',#19056);
#5827=VERTEX_POINT('',#19060);
#5828=VERTEX_POINT('',#19064);
#5829=VERTEX_POINT('',#19068);
#5830=VERTEX_POINT('',#19072);
#5831=VERTEX_POINT('',#19076);
#5832=VERTEX_POINT('',#19087);
#5833=VERTEX_POINT('',#19088);
#5834=VERTEX_POINT('',#19090);
#5835=VERTEX_POINT('',#19092);
#5836=VERTEX_POINT('',#19096);
#5837=VERTEX_POINT('',#19097);
#5838=VERTEX_POINT('',#19102);
#5839=VERTEX_POINT('',#19103);
#5840=VERTEX_POINT('',#19111);
#5841=VERTEX_POINT('',#19113);
#5842=VERTEX_POINT('',#19117);
#5843=VERTEX_POINT('',#19122);
#5844=VERTEX_POINT('',#19124);
#5845=VERTEX_POINT('',#19128);
#5846=VERTEX_POINT('',#19132);
#5847=VERTEX_POINT('',#19133);
#5848=VERTEX_POINT('',#19146);
#5849=VERTEX_POINT('',#19147);
#5850=VERTEX_POINT('',#19149);
#5851=VERTEX_POINT('',#19151);
#5852=VERTEX_POINT('',#19155);
#5853=VERTEX_POINT('',#19157);
#5854=VERTEX_POINT('',#19161);
#5855=VERTEX_POINT('',#19163);
#5856=VERTEX_POINT('',#19167);
#5857=VERTEX_POINT('',#19169);
#5858=VERTEX_POINT('',#19173);
#5859=VERTEX_POINT('',#19175);
#5860=VERTEX_POINT('',#19183);
#5861=VERTEX_POINT('',#19186);
#5862=VERTEX_POINT('',#19190);
#5863=VERTEX_POINT('',#19194);
#5864=VERTEX_POINT('',#19200);
#5865=VERTEX_POINT('',#19203);
#5866=VERTEX_POINT('',#19207);
#5867=VERTEX_POINT('',#19211);
#5868=VERTEX_POINT('',#19215);
#5869=VERTEX_POINT('',#19218);
#5870=VERTEX_POINT('',#19222);
#5871=VERTEX_POINT('',#19226);
#5872=VERTEX_POINT('',#19231);
#5873=VERTEX_POINT('',#19232);
#5874=VERTEX_POINT('',#19234);
#5875=VERTEX_POINT('',#19236);
#5876=VERTEX_POINT('',#19240);
#5877=VERTEX_POINT('',#19242);
#5878=VERTEX_POINT('',#19246);
#5879=VERTEX_POINT('',#19248);
#5880=VERTEX_POINT('',#19252);
#5881=VERTEX_POINT('',#19254);
#5882=VERTEX_POINT('',#19258);
#5883=VERTEX_POINT('',#19260);
#5884=EDGE_CURVE('',#4943,#4943,#4681,.T.);
#5885=EDGE_CURVE('',#4943,#4944,#2375,.T.);
#5886=EDGE_CURVE('',#4944,#4944,#4682,.T.);
#5887=EDGE_CURVE('',#4945,#4945,#4683,.T.);
#5888=EDGE_CURVE('',#4945,#4946,#2376,.T.);
#5889=EDGE_CURVE('',#4946,#4946,#4684,.T.);
#5890=EDGE_CURVE('',#4947,#4947,#4685,.T.);
#5891=EDGE_CURVE('',#4947,#4948,#2377,.T.);
#5892=EDGE_CURVE('',#4948,#4948,#4686,.T.);
#5893=EDGE_CURVE('',#4949,#4949,#4687,.T.);
#5894=EDGE_CURVE('',#4949,#4950,#2378,.T.);
#5895=EDGE_CURVE('',#4950,#4950,#4688,.T.);
#5896=EDGE_CURVE('',#4951,#4951,#4689,.T.);
#5897=EDGE_CURVE('',#4951,#4952,#2379,.T.);
#5898=EDGE_CURVE('',#4952,#4952,#4690,.T.);
#5899=EDGE_CURVE('',#4953,#4953,#4691,.T.);
#5900=EDGE_CURVE('',#4953,#4954,#2380,.T.);
#5901=EDGE_CURVE('',#4954,#4954,#4692,.T.);
#5902=EDGE_CURVE('',#4955,#4956,#2381,.T.);
#5903=EDGE_CURVE('',#4956,#4957,#2382,.T.);
#5904=EDGE_CURVE('',#4958,#4957,#2383,.T.);
#5905=EDGE_CURVE('',#4955,#4958,#2384,.T.);
#5906=EDGE_CURVE('',#4959,#4955,#2385,.T.);
#5907=EDGE_CURVE('',#4960,#4958,#2386,.T.);
#5908=EDGE_CURVE('',#4959,#4960,#2387,.T.);
#5909=EDGE_CURVE('',#4961,#4959,#2388,.T.);
#5910=EDGE_CURVE('',#4962,#4960,#2389,.T.);
#5911=EDGE_CURVE('',#4961,#4962,#2390,.T.);
#5912=EDGE_CURVE('',#4956,#4961,#2391,.T.);
#5913=EDGE_CURVE('',#4957,#4962,#2392,.T.);
#5914=EDGE_CURVE('',#4963,#4964,#2393,.T.);
#5915=EDGE_CURVE('',#4964,#4965,#2394,.T.);
#5916=EDGE_CURVE('',#4966,#4965,#2395,.T.);
#5917=EDGE_CURVE('',#4963,#4966,#2396,.T.);
#5918=EDGE_CURVE('',#4967,#4963,#2397,.T.);
#5919=EDGE_CURVE('',#4968,#4966,#2398,.T.);
#5920=EDGE_CURVE('',#4967,#4968,#2399,.T.);
#5921=EDGE_CURVE('',#4969,#4967,#2400,.T.);
#5922=EDGE_CURVE('',#4970,#4968,#2401,.T.);
#5923=EDGE_CURVE('',#4969,#4970,#2402,.T.);
#5924=EDGE_CURVE('',#4964,#4969,#2403,.T.);
#5925=EDGE_CURVE('',#4965,#4970,#2404,.T.);
#5926=EDGE_CURVE('',#4971,#4972,#2405,.T.);
#5927=EDGE_CURVE('',#4972,#4973,#2406,.T.);
#5928=EDGE_CURVE('',#4974,#4973,#2407,.T.);
#5929=EDGE_CURVE('',#4971,#4974,#2408,.T.);
#5930=EDGE_CURVE('',#4975,#4971,#2409,.T.);
#5931=EDGE_CURVE('',#4976,#4974,#2410,.T.);
#5932=EDGE_CURVE('',#4975,#4976,#2411,.T.);
#5933=EDGE_CURVE('',#4977,#4975,#2412,.T.);
#5934=EDGE_CURVE('',#4978,#4976,#2413,.T.);
#5935=EDGE_CURVE('',#4977,#4978,#2414,.T.);
#5936=EDGE_CURVE('',#4972,#4977,#2415,.T.);
#5937=EDGE_CURVE('',#4973,#4978,#2416,.T.);
#5938=EDGE_CURVE('',#4979,#4979,#4693,.T.);
#5939=EDGE_CURVE('',#4979,#4980,#2417,.T.);
#5940=EDGE_CURVE('',#4980,#4980,#4694,.T.);
#5941=EDGE_CURVE('',#4981,#4981,#4695,.T.);
#5942=EDGE_CURVE('',#4981,#4982,#2418,.T.);
#5943=EDGE_CURVE('',#4982,#4982,#4696,.T.);
#5944=EDGE_CURVE('',#4983,#4983,#4697,.T.);
#5945=EDGE_CURVE('',#4983,#4984,#2419,.T.);
#5946=EDGE_CURVE('',#4984,#4984,#4698,.T.);
#5947=EDGE_CURVE('',#4985,#4985,#4699,.T.);
#5948=EDGE_CURVE('',#4985,#4986,#2420,.T.);
#5949=EDGE_CURVE('',#4986,#4986,#4700,.T.);
#5950=EDGE_CURVE('',#4987,#4987,#4701,.T.);
#5951=EDGE_CURVE('',#4987,#4988,#2421,.T.);
#5952=EDGE_CURVE('',#4988,#4988,#4702,.T.);
#5953=EDGE_CURVE('',#4989,#4989,#4703,.T.);
#5954=EDGE_CURVE('',#4989,#4990,#2422,.T.);
#5955=EDGE_CURVE('',#4990,#4990,#4704,.T.);
#5956=EDGE_CURVE('',#4991,#4991,#4705,.T.);
#5957=EDGE_CURVE('',#4991,#4992,#2423,.T.);
#5958=EDGE_CURVE('',#4992,#4992,#4706,.T.);
#5959=EDGE_CURVE('',#4993,#4993,#4707,.T.);
#5960=EDGE_CURVE('',#4993,#4994,#2424,.T.);
#5961=EDGE_CURVE('',#4994,#4994,#4708,.T.);
#5962=EDGE_CURVE('',#4995,#4995,#4709,.T.);
#5963=EDGE_CURVE('',#4995,#4996,#2425,.T.);
#5964=EDGE_CURVE('',#4996,#4996,#4710,.T.);
#5965=EDGE_CURVE('',#4997,#4997,#4711,.T.);
#5966=EDGE_CURVE('',#4997,#4998,#2426,.T.);
#5967=EDGE_CURVE('',#4998,#4998,#4712,.T.);
#5968=EDGE_CURVE('',#4999,#4999,#4713,.T.);
#5969=EDGE_CURVE('',#4999,#5000,#2427,.T.);
#5970=EDGE_CURVE('',#5000,#5000,#4714,.T.);
#5971=EDGE_CURVE('',#5001,#5001,#4715,.T.);
#5972=EDGE_CURVE('',#5001,#5002,#2428,.T.);
#5973=EDGE_CURVE('',#5002,#5002,#4716,.T.);
#5974=EDGE_CURVE('',#5003,#5003,#4717,.T.);
#5975=EDGE_CURVE('',#5003,#5004,#2429,.T.);
#5976=EDGE_CURVE('',#5004,#5004,#4718,.T.);
#5977=EDGE_CURVE('',#5005,#5005,#4719,.T.);
#5978=EDGE_CURVE('',#5005,#5006,#2430,.T.);
#5979=EDGE_CURVE('',#5006,#5006,#4720,.T.);
#5980=EDGE_CURVE('',#5007,#5007,#4721,.T.);
#5981=EDGE_CURVE('',#5007,#5008,#2431,.T.);
#5982=EDGE_CURVE('',#5008,#5008,#4722,.T.);
#5983=EDGE_CURVE('',#5009,#5010,#2432,.T.);
#5984=EDGE_CURVE('',#5011,#5009,#2433,.T.);
#5985=EDGE_CURVE('',#5012,#5011,#2434,.T.);
#5986=EDGE_CURVE('',#5012,#5010,#2435,.T.);
#5987=EDGE_CURVE('',#5011,#5013,#2436,.T.);
#5988=EDGE_CURVE('',#5013,#5014,#2437,.T.);
#5989=EDGE_CURVE('',#5014,#5012,#2438,.T.);
#5990=EDGE_CURVE('',#5015,#5016,#2439,.T.);
#5991=EDGE_CURVE('',#5017,#5016,#2440,.T.);
#5992=EDGE_CURVE('',#5018,#5017,#2441,.T.);
#5993=EDGE_CURVE('',#5018,#5015,#2442,.T.);
#5994=EDGE_CURVE('',#5009,#5019,#2443,.T.);
#5995=EDGE_CURVE('',#5016,#5019,#2444,.T.);
#5996=EDGE_CURVE('',#5015,#5013,#2445,.T.);
#5997=EDGE_CURVE('',#5020,#5017,#2446,.T.);
#5998=EDGE_CURVE('',#5010,#5020,#2447,.T.);
#5999=EDGE_CURVE('',#5014,#5018,#2448,.T.);
#6000=EDGE_CURVE('',#5019,#5020,#2449,.T.);
#6001=EDGE_CURVE('',#5021,#5021,#4723,.T.);
#6002=EDGE_CURVE('',#5021,#5022,#2450,.T.);
#6003=EDGE_CURVE('',#5022,#5022,#4724,.T.);
#6004=EDGE_CURVE('',#5023,#5023,#4725,.T.);
#6005=EDGE_CURVE('',#5023,#5024,#2451,.T.);
#6006=EDGE_CURVE('',#5024,#5024,#4726,.T.);
#6007=EDGE_CURVE('',#5025,#5025,#4727,.T.);
#6008=EDGE_CURVE('',#5025,#5026,#2452,.T.);
#6009=EDGE_CURVE('',#5026,#5026,#4728,.T.);
#6010=EDGE_CURVE('',#5027,#5027,#4729,.T.);
#6011=EDGE_CURVE('',#5027,#5028,#2453,.T.);
#6012=EDGE_CURVE('',#5028,#5028,#4730,.T.);
#6013=EDGE_CURVE('',#5029,#5029,#4731,.T.);
#6014=EDGE_CURVE('',#5029,#5030,#2454,.T.);
#6015=EDGE_CURVE('',#5030,#5030,#4732,.T.);
#6016=EDGE_CURVE('',#5031,#5031,#4733,.T.);
#6017=EDGE_CURVE('',#5032,#5032,#4734,.T.);
#6018=EDGE_CURVE('',#5032,#5031,#2455,.T.);
#6019=EDGE_CURVE('',#5033,#5034,#2456,.T.);
#6020=EDGE_CURVE('',#5034,#5035,#2457,.T.);
#6021=EDGE_CURVE('',#5036,#5035,#2458,.T.);
#6022=EDGE_CURVE('',#5033,#5036,#2459,.T.);
#6023=EDGE_CURVE('',#5037,#5033,#2460,.T.);
#6024=EDGE_CURVE('',#5038,#5036,#2461,.T.);
#6025=EDGE_CURVE('',#5037,#5038,#2462,.T.);
#6026=EDGE_CURVE('',#5039,#5037,#2463,.T.);
#6027=EDGE_CURVE('',#5040,#5038,#2464,.T.);
#6028=EDGE_CURVE('',#5039,#5040,#2465,.T.);
#6029=EDGE_CURVE('',#5034,#5039,#2466,.T.);
#6030=EDGE_CURVE('',#5035,#5040,#2467,.T.);
#6031=EDGE_CURVE('',#5041,#5042,#2468,.T.);
#6032=EDGE_CURVE('',#5043,#5041,#2469,.T.);
#6033=EDGE_CURVE('',#5043,#5044,#2470,.T.);
#6034=EDGE_CURVE('',#5044,#5042,#2471,.T.);
#6035=EDGE_CURVE('',#5042,#5045,#2472,.T.);
#6036=EDGE_CURVE('',#5044,#5046,#2473,.T.);
#6037=EDGE_CURVE('',#5046,#5045,#2474,.T.);
#6038=EDGE_CURVE('',#5045,#5047,#2475,.T.);
#6039=EDGE_CURVE('',#5046,#5048,#2476,.T.);
#6040=EDGE_CURVE('',#5048,#5047,#2477,.T.);
#6041=EDGE_CURVE('',#5047,#5049,#2478,.T.);
#6042=EDGE_CURVE('',#5048,#5050,#2479,.T.);
#6043=EDGE_CURVE('',#5050,#5049,#2480,.T.);
#6044=EDGE_CURVE('',#5049,#5051,#2481,.T.);
#6045=EDGE_CURVE('',#5050,#5052,#2482,.T.);
#6046=EDGE_CURVE('',#5052,#5051,#2483,.T.);
#6047=EDGE_CURVE('',#5051,#5041,#2484,.T.);
#6048=EDGE_CURVE('',#5052,#5043,#2485,.T.);
#6049=EDGE_CURVE('',#5053,#5053,#4735,.T.);
#6050=EDGE_CURVE('',#5054,#5054,#4736,.T.);
#6051=EDGE_CURVE('',#5055,#5055,#4737,.T.);
#6052=EDGE_CURVE('',#5055,#5053,#2486,.T.);
#6053=EDGE_CURVE('',#5054,#5056,#2487,.T.);
#6054=EDGE_CURVE('',#5056,#5056,#4738,.T.);
#6055=EDGE_CURVE('',#5057,#5058,#2488,.T.);
#6056=EDGE_CURVE('',#5059,#5057,#2489,.T.);
#6057=EDGE_CURVE('',#5059,#5060,#2490,.T.);
#6058=EDGE_CURVE('',#5060,#5058,#2491,.T.);
#6059=EDGE_CURVE('',#5058,#5061,#2492,.T.);
#6060=EDGE_CURVE('',#5060,#5062,#2493,.T.);
#6061=EDGE_CURVE('',#5062,#5061,#2494,.T.);
#6062=EDGE_CURVE('',#5061,#5063,#2495,.T.);
#6063=EDGE_CURVE('',#5062,#5064,#2496,.T.);
#6064=EDGE_CURVE('',#5064,#5063,#2497,.T.);
#6065=EDGE_CURVE('',#5063,#5065,#2498,.T.);
#6066=EDGE_CURVE('',#5064,#5066,#2499,.T.);
#6067=EDGE_CURVE('',#5066,#5065,#2500,.T.);
#6068=EDGE_CURVE('',#5065,#5067,#2501,.T.);
#6069=EDGE_CURVE('',#5066,#5068,#2502,.T.);
#6070=EDGE_CURVE('',#5068,#5067,#2503,.T.);
#6071=EDGE_CURVE('',#5067,#5057,#2504,.T.);
#6072=EDGE_CURVE('',#5068,#5059,#2505,.T.);
#6073=EDGE_CURVE('',#5069,#5069,#4739,.T.);
#6074=EDGE_CURVE('',#5070,#5070,#4740,.T.);
#6075=EDGE_CURVE('',#5071,#5071,#4741,.T.);
#6076=EDGE_CURVE('',#5071,#5069,#2506,.T.);
#6077=EDGE_CURVE('',#5070,#5072,#2507,.T.);
#6078=EDGE_CURVE('',#5072,#5072,#4742,.T.);
#6079=EDGE_CURVE('',#5073,#5074,#2508,.T.);
#6080=EDGE_CURVE('',#5075,#5073,#2509,.T.);
#6081=EDGE_CURVE('',#5075,#5076,#2510,.T.);
#6082=EDGE_CURVE('',#5076,#5074,#2511,.T.);
#6083=EDGE_CURVE('',#5074,#5077,#2512,.T.);
#6084=EDGE_CURVE('',#5076,#5078,#2513,.T.);
#6085=EDGE_CURVE('',#5078,#5077,#2514,.T.);
#6086=EDGE_CURVE('',#5077,#5079,#2515,.T.);
#6087=EDGE_CURVE('',#5078,#5080,#2516,.T.);
#6088=EDGE_CURVE('',#5080,#5079,#2517,.T.);
#6089=EDGE_CURVE('',#5079,#5081,#2518,.T.);
#6090=EDGE_CURVE('',#5080,#5082,#2519,.T.);
#6091=EDGE_CURVE('',#5082,#5081,#2520,.T.);
#6092=EDGE_CURVE('',#5081,#5083,#2521,.T.);
#6093=EDGE_CURVE('',#5082,#5084,#2522,.T.);
#6094=EDGE_CURVE('',#5084,#5083,#2523,.T.);
#6095=EDGE_CURVE('',#5083,#5073,#2524,.T.);
#6096=EDGE_CURVE('',#5084,#5075,#2525,.T.);
#6097=EDGE_CURVE('',#5085,#5085,#4743,.T.);
#6098=EDGE_CURVE('',#5086,#5086,#4744,.T.);
#6099=EDGE_CURVE('',#5087,#5087,#4745,.T.);
#6100=EDGE_CURVE('',#5087,#5085,#2526,.T.);
#6101=EDGE_CURVE('',#5086,#5088,#2527,.T.);
#6102=EDGE_CURVE('',#5088,#5088,#4746,.T.);
#6103=EDGE_CURVE('',#5089,#5090,#2528,.T.);
#6104=EDGE_CURVE('',#5091,#5089,#2529,.T.);
#6105=EDGE_CURVE('',#5091,#5092,#2530,.T.);
#6106=EDGE_CURVE('',#5092,#5090,#2531,.T.);
#6107=EDGE_CURVE('',#5090,#5093,#2532,.T.);
#6108=EDGE_CURVE('',#5092,#5094,#2533,.T.);
#6109=EDGE_CURVE('',#5094,#5093,#2534,.T.);
#6110=EDGE_CURVE('',#5093,#5095,#2535,.T.);
#6111=EDGE_CURVE('',#5094,#5096,#2536,.T.);
#6112=EDGE_CURVE('',#5096,#5095,#2537,.T.);
#6113=EDGE_CURVE('',#5095,#5097,#2538,.T.);
#6114=EDGE_CURVE('',#5096,#5098,#2539,.T.);
#6115=EDGE_CURVE('',#5098,#5097,#2540,.T.);
#6116=EDGE_CURVE('',#5097,#5099,#2541,.T.);
#6117=EDGE_CURVE('',#5098,#5100,#2542,.T.);
#6118=EDGE_CURVE('',#5100,#5099,#2543,.T.);
#6119=EDGE_CURVE('',#5099,#5089,#2544,.T.);
#6120=EDGE_CURVE('',#5100,#5091,#2545,.T.);
#6121=EDGE_CURVE('',#5101,#5101,#4747,.T.);
#6122=EDGE_CURVE('',#5102,#5102,#4748,.T.);
#6123=EDGE_CURVE('',#5103,#5103,#4749,.T.);
#6124=EDGE_CURVE('',#5103,#5101,#2546,.T.);
#6125=EDGE_CURVE('',#5102,#5104,#2547,.T.);
#6126=EDGE_CURVE('',#5104,#5104,#4750,.T.);
#6127=EDGE_CURVE('',#5105,#5106,#2548,.T.);
#6128=EDGE_CURVE('',#5106,#5105,#4751,.T.);
#6129=EDGE_CURVE('',#5107,#5108,#2549,.T.);
#6130=EDGE_CURVE('',#5107,#5109,#4752,.T.);
#6131=EDGE_CURVE('',#5110,#5109,#2550,.T.);
#6132=EDGE_CURVE('',#5111,#5110,#4753,.T.);
#6133=EDGE_CURVE('',#5111,#5112,#2551,.T.);
#6134=EDGE_CURVE('',#5112,#5112,#4754,.T.);
#6135=EDGE_CURVE('',#5108,#5111,#4755,.T.);
#6136=EDGE_CURVE('',#5113,#5113,#4756,.T.);
#6137=EDGE_CURVE('',#5113,#5114,#2552,.T.);
#6138=EDGE_CURVE('',#5115,#5114,#4757,.T.);
#6139=EDGE_CURVE('',#5106,#5115,#2553,.T.);
#6140=EDGE_CURVE('',#5116,#5105,#2554,.T.);
#6141=EDGE_CURVE('',#5114,#5116,#4758,.T.);
#6142=EDGE_CURVE('',#5109,#5107,#2555,.T.);
#6143=EDGE_CURVE('',#5117,#5110,#2556,.T.);
#6144=EDGE_CURVE('',#5117,#5118,#4759,.T.);
#6145=EDGE_CURVE('',#5108,#5118,#2557,.T.);
#6146=EDGE_CURVE('',#5119,#5120,#4760,.T.);
#6147=EDGE_CURVE('',#5121,#5122,#2558,.T.);
#6148=EDGE_CURVE('',#5121,#5123,#2559,.T.);
#6149=EDGE_CURVE('',#5122,#5123,#4761,.T.);
#6150=EDGE_CURVE('',#5124,#5125,#2560,.T.);
#6151=EDGE_CURVE('',#5126,#5124,#4762,.T.);
#6152=EDGE_CURVE('',#5126,#5125,#2561,.T.);
#6153=EDGE_CURVE('',#5127,#5128,#2562,.T.);
#6154=EDGE_CURVE('',#5129,#5127,#4763,.T.);
#6155=EDGE_CURVE('',#5129,#5128,#2563,.T.);
#6156=EDGE_CURVE('',#5128,#5121,#2564,.T.);
#6157=EDGE_CURVE('',#5123,#5129,#2565,.T.);
#6158=EDGE_CURVE('',#5130,#5131,#2566,.T.);
#6159=EDGE_CURVE('',#5130,#5132,#2567,.T.);
#6160=EDGE_CURVE('',#5131,#5132,#4764,.T.);
#6161=EDGE_CURVE('',#5125,#5130,#2568,.T.);
#6162=EDGE_CURVE('',#5132,#5126,#2569,.T.);
#6163=EDGE_CURVE('',#5133,#5134,#2570,.T.);
#6164=EDGE_CURVE('',#5134,#5135,#2571,.T.);
#6165=EDGE_CURVE('',#5135,#5136,#2572,.T.);
#6166=EDGE_CURVE('',#5136,#5133,#2573,.T.);
#6167=EDGE_CURVE('',#5118,#5127,#2574,.T.);
#6168=EDGE_CURVE('',#5122,#5137,#2575,.T.);
#6169=EDGE_CURVE('',#5137,#5116,#2576,.T.);
#6170=EDGE_CURVE('',#5115,#5138,#2577,.T.);
#6171=EDGE_CURVE('',#5138,#5124,#2578,.T.);
#6172=EDGE_CURVE('',#5131,#5117,#2579,.T.);
#6173=EDGE_CURVE('',#5139,#5139,#4765,.T.);
#6174=EDGE_CURVE('',#5140,#5140,#4766,.T.);
#6175=EDGE_CURVE('',#5141,#5142,#4767,.T.);
#6176=EDGE_CURVE('',#5143,#5141,#2580,.T.);
#6177=EDGE_CURVE('',#5144,#5143,#4768,.T.);
#6178=EDGE_CURVE('',#5142,#5144,#2581,.T.);
#6179=EDGE_CURVE('',#5137,#5138,#4769,.T.);
#6180=EDGE_CURVE('',#5143,#5145,#2582,.T.);
#6181=EDGE_CURVE('',#5146,#5145,#2583,.T.);
#6182=EDGE_CURVE('',#5147,#5146,#2584,.T.);
#6183=EDGE_CURVE('',#5147,#5148,#2585,.T.);
#6184=EDGE_CURVE('',#5148,#5144,#2586,.T.);
#6185=EDGE_CURVE('',#5149,#5141,#2587,.T.);
#6186=EDGE_CURVE('',#5145,#5149,#2588,.T.);
#6187=EDGE_CURVE('',#5150,#5147,#2589,.T.);
#6188=EDGE_CURVE('',#5150,#5151,#2590,.T.);
#6189=EDGE_CURVE('',#5151,#5148,#2591,.T.);
#6190=EDGE_CURVE('',#5142,#5151,#2592,.T.);
#6191=EDGE_CURVE('',#5152,#5150,#2593,.T.);
#6192=EDGE_CURVE('',#5152,#5149,#2594,.T.);
#6193=EDGE_CURVE('',#5146,#5152,#2595,.T.);
#6194=EDGE_CURVE('',#5153,#5153,#4770,.T.);
#6195=EDGE_CURVE('',#5153,#5140,#2596,.T.);
#6196=EDGE_CURVE('',#5154,#5154,#4771,.T.);
#6197=EDGE_CURVE('',#5154,#5139,#2597,.T.);
#6198=EDGE_CURVE('',#5155,#5156,#2598,.T.);
#6199=EDGE_CURVE('',#5156,#5133,#2599,.T.);
#6200=EDGE_CURVE('',#5155,#5136,#2600,.T.);
#6201=EDGE_CURVE('',#5157,#5155,#2601,.T.);
#6202=EDGE_CURVE('',#5157,#5135,#2602,.T.);
#6203=EDGE_CURVE('',#5158,#5157,#2603,.T.);
#6204=EDGE_CURVE('',#5158,#5134,#2604,.T.);
#6205=EDGE_CURVE('',#5156,#5158,#2605,.T.);
#6206=EDGE_CURVE('',#5159,#5159,#4772,.T.);
#6207=EDGE_CURVE('',#5159,#5160,#2606,.T.);
#6208=EDGE_CURVE('',#5160,#5160,#4773,.T.);
#6209=EDGE_CURVE('',#5161,#5161,#4774,.T.);
#6210=EDGE_CURVE('',#5162,#5163,#4775,.T.);
#6211=EDGE_CURVE('',#5164,#5164,#4776,.T.);
#6212=EDGE_CURVE('',#5165,#5166,#227,.T.);
#6213=EDGE_CURVE('',#5167,#5165,#228,.T.);
#6214=EDGE_CURVE('',#5166,#5167,#229,.T.);
#6215=EDGE_CURVE('',#5166,#5168,#2607,.T.);
#6216=EDGE_CURVE('',#5168,#5168,#230,.T.);
#6217=EDGE_CURVE('',#5169,#5169,#231,.T.);
#6218=EDGE_CURVE('',#5169,#5170,#2608,.T.);
#6219=EDGE_CURVE('',#5171,#5170,#232,.T.);
#6220=EDGE_CURVE('',#5172,#5171,#233,.T.);
#6221=EDGE_CURVE('',#5170,#5172,#234,.T.);
#6222=EDGE_CURVE('',#5173,#5173,#4777,.T.);
#6223=EDGE_CURVE('',#5173,#5174,#2609,.T.);
#6224=EDGE_CURVE('',#5174,#5174,#4778,.T.);
#6225=EDGE_CURVE('',#5175,#5176,#235,.T.);
#6226=EDGE_CURVE('',#5176,#5177,#236,.T.);
#6227=EDGE_CURVE('',#5177,#5175,#237,.T.);
#6228=EDGE_CURVE('',#5178,#5179,#238,.T.);
#6229=EDGE_CURVE('',#5179,#5180,#239,.T.);
#6230=EDGE_CURVE('',#5180,#5178,#240,.T.);
#6231=EDGE_CURVE('',#5181,#5182,#241,.T.);
#6232=EDGE_CURVE('',#5182,#5183,#242,.T.);
#6233=EDGE_CURVE('',#5183,#5181,#243,.T.);
#6234=EDGE_CURVE('',#5184,#5185,#244,.T.);
#6235=EDGE_CURVE('',#5185,#5186,#245,.T.);
#6236=EDGE_CURVE('',#5186,#5184,#246,.T.);
#6237=EDGE_CURVE('',#5177,#5187,#2610,.T.);
#6238=EDGE_CURVE('',#5187,#5187,#247,.T.);
#6239=EDGE_CURVE('',#5188,#5188,#248,.T.);
#6240=EDGE_CURVE('',#5188,#5180,#2611,.T.);
#6241=EDGE_CURVE('',#5183,#5189,#2612,.T.);
#6242=EDGE_CURVE('',#5189,#5189,#249,.T.);
#6243=EDGE_CURVE('',#5190,#5190,#250,.T.);
#6244=EDGE_CURVE('',#5190,#5186,#2613,.T.);
#6245=EDGE_CURVE('',#5191,#5191,#4779,.T.);
#6246=EDGE_CURVE('',#5192,#5192,#4780,.T.);
#6247=EDGE_CURVE('',#5193,#5193,#4781,.T.);
#6248=EDGE_CURVE('',#5193,#5192,#2614,.T.);
#6249=EDGE_CURVE('',#5194,#5194,#4782,.T.);
#6250=EDGE_CURVE('',#5194,#5191,#2615,.T.);
#6251=EDGE_CURVE('',#5195,#5195,#4783,.T.);
#6252=EDGE_CURVE('',#5195,#5196,#2616,.T.);
#6253=EDGE_CURVE('',#5196,#5196,#4784,.T.);
#6254=EDGE_CURVE('',#5197,#5197,#4785,.T.);
#6255=EDGE_CURVE('',#5197,#5198,#2617,.T.);
#6256=EDGE_CURVE('',#5198,#5198,#4786,.T.);
#6257=EDGE_CURVE('',#5199,#5200,#2618,.T.);
#6258=EDGE_CURVE('',#5200,#5201,#2619,.T.);
#6259=EDGE_CURVE('',#5201,#5202,#2620,.T.);
#6260=EDGE_CURVE('',#5199,#5202,#2621,.T.);
#6261=EDGE_CURVE('',#5200,#5203,#2622,.T.);
#6262=EDGE_CURVE('',#5203,#5204,#2623,.T.);
#6263=EDGE_CURVE('',#5204,#5201,#2624,.T.);
#6264=EDGE_CURVE('',#5203,#5205,#2625,.T.);
#6265=EDGE_CURVE('',#5205,#5206,#2626,.T.);
#6266=EDGE_CURVE('',#5206,#5204,#2627,.T.);
#6267=EDGE_CURVE('',#5205,#5207,#2628,.T.);
#6268=EDGE_CURVE('',#5207,#5208,#2629,.T.);
#6269=EDGE_CURVE('',#5208,#5206,#2630,.T.);
#6270=EDGE_CURVE('',#5207,#5209,#2631,.T.);
#6271=EDGE_CURVE('',#5209,#5210,#2632,.T.);
#6272=EDGE_CURVE('',#5210,#5208,#2633,.T.);
#6273=EDGE_CURVE('',#5209,#5199,#2634,.T.);
#6274=EDGE_CURVE('',#5202,#5210,#2635,.T.);
#6275=EDGE_CURVE('',#5211,#5211,#4787,.T.);
#6276=EDGE_CURVE('',#5212,#5212,#4788,.T.);
#6277=EDGE_CURVE('',#5213,#5213,#4789,.T.);
#6278=EDGE_CURVE('',#5213,#5212,#2636,.T.);
#6279=EDGE_CURVE('',#5214,#5214,#4790,.T.);
#6280=EDGE_CURVE('',#5214,#5213,#2637,.T.);
#6281=EDGE_CURVE('',#5215,#5215,#4791,.T.);
#6282=EDGE_CURVE('',#5215,#5214,#2638,.T.);
#6283=EDGE_CURVE('',#5216,#5216,#4792,.T.);
#6284=EDGE_CURVE('',#5217,#5217,#4793,.F.);
#6285=EDGE_CURVE('',#5217,#5216,#2639,.T.);
#6286=EDGE_CURVE('',#5211,#5217,#2640,.T.);
#6287=EDGE_CURVE('',#5218,#5219,#2641,.T.);
#6288=EDGE_CURVE('',#5219,#5220,#2642,.T.);
#6289=EDGE_CURVE('',#5220,#5221,#2643,.T.);
#6290=EDGE_CURVE('',#5218,#5221,#2644,.T.);
#6291=EDGE_CURVE('',#5219,#5222,#2645,.T.);
#6292=EDGE_CURVE('',#5222,#5223,#2646,.T.);
#6293=EDGE_CURVE('',#5223,#5220,#2647,.T.);
#6294=EDGE_CURVE('',#5222,#5224,#2648,.T.);
#6295=EDGE_CURVE('',#5224,#5225,#2649,.T.);
#6296=EDGE_CURVE('',#5225,#5223,#2650,.T.);
#6297=EDGE_CURVE('',#5224,#5226,#2651,.T.);
#6298=EDGE_CURVE('',#5226,#5227,#2652,.T.);
#6299=EDGE_CURVE('',#5227,#5225,#2653,.T.);
#6300=EDGE_CURVE('',#5226,#5228,#2654,.T.);
#6301=EDGE_CURVE('',#5228,#5229,#2655,.T.);
#6302=EDGE_CURVE('',#5229,#5227,#2656,.T.);
#6303=EDGE_CURVE('',#5228,#5218,#2657,.T.);
#6304=EDGE_CURVE('',#5221,#5229,#2658,.T.);
#6305=EDGE_CURVE('',#5230,#5230,#4794,.T.);
#6306=EDGE_CURVE('',#5231,#5231,#4795,.T.);
#6307=EDGE_CURVE('',#5232,#5232,#4796,.T.);
#6308=EDGE_CURVE('',#5232,#5231,#2659,.T.);
#6309=EDGE_CURVE('',#5233,#5233,#4797,.T.);
#6310=EDGE_CURVE('',#5233,#5232,#2660,.T.);
#6311=EDGE_CURVE('',#5234,#5234,#4798,.T.);
#6312=EDGE_CURVE('',#5234,#5233,#2661,.T.);
#6313=EDGE_CURVE('',#5235,#5235,#4799,.T.);
#6314=EDGE_CURVE('',#5236,#5236,#4800,.F.);
#6315=EDGE_CURVE('',#5236,#5235,#2662,.T.);
#6316=EDGE_CURVE('',#5230,#5236,#2663,.T.);
#6317=EDGE_CURVE('',#5237,#5238,#2664,.T.);
#6318=EDGE_CURVE('',#5237,#5239,#2665,.T.);
#6319=EDGE_CURVE('',#5240,#5239,#2666,.T.);
#6320=EDGE_CURVE('',#5240,#5238,#2667,.T.);
#6321=EDGE_CURVE('',#5238,#5241,#4801,.T.);
#6322=EDGE_CURVE('',#5242,#5240,#2668,.T.);
#6323=EDGE_CURVE('',#5241,#5242,#2669,.T.);
#6324=EDGE_CURVE('',#5241,#5243,#2670,.T.);
#6325=EDGE_CURVE('',#5242,#5244,#2671,.T.);
#6326=EDGE_CURVE('',#5244,#5243,#2672,.T.);
#6327=EDGE_CURVE('',#5239,#5244,#2673,.T.);
#6328=EDGE_CURVE('',#5243,#5237,#4802,.T.);
#6329=EDGE_CURVE('',#5245,#5245,#4803,.T.);
#6330=EDGE_CURVE('',#5245,#5246,#2674,.T.);
#6331=EDGE_CURVE('',#5246,#5246,#4804,.T.);
#6332=EDGE_CURVE('',#5247,#5247,#4805,.T.);
#6333=EDGE_CURVE('',#5247,#5248,#2675,.T.);
#6334=EDGE_CURVE('',#5248,#5248,#4806,.T.);
#6335=EDGE_CURVE('',#5249,#5249,#4807,.T.);
#6336=EDGE_CURVE('',#5249,#5250,#2676,.T.);
#6337=EDGE_CURVE('',#5250,#5250,#4808,.T.);
#6338=EDGE_CURVE('',#5251,#5252,#2677,.T.);
#6339=EDGE_CURVE('',#5251,#5252,#4809,.T.);
#6340=EDGE_CURVE('',#5253,#5251,#251,.T.);
#6341=EDGE_CURVE('',#5254,#5253,#4810,.T.);
#6342=EDGE_CURVE('',#5254,#5255,#2678,.T.);
#6343=EDGE_CURVE('',#5256,#5255,#252,.T.);
#6344=EDGE_CURVE('',#5255,#5256,#253,.T.);
#6345=EDGE_CURVE('',#5257,#5254,#4811,.T.);
#6346=EDGE_CURVE('',#5252,#5257,#254,.T.);
#6347=EDGE_CURVE('',#5257,#5253,#2679,.T.);
#6348=EDGE_CURVE('',#5258,#5258,#4812,.T.);
#6349=EDGE_CURVE('',#5258,#5259,#2680,.T.);
#6350=EDGE_CURVE('',#5259,#5259,#4813,.T.);
#6351=EDGE_CURVE('',#5260,#5260,#4814,.T.);
#6352=EDGE_CURVE('',#5260,#5261,#2681,.T.);
#6353=EDGE_CURVE('',#5261,#5261,#4815,.T.);
#6354=EDGE_CURVE('',#5262,#5263,#2682,.T.);
#6355=EDGE_CURVE('',#5262,#5263,#4816,.T.);
#6356=EDGE_CURVE('',#5264,#5262,#255,.T.);
#6357=EDGE_CURVE('',#5265,#5264,#4817,.T.);
#6358=EDGE_CURVE('',#5265,#5266,#2683,.T.);
#6359=EDGE_CURVE('',#5267,#5266,#256,.T.);
#6360=EDGE_CURVE('',#5266,#5267,#257,.T.);
#6361=EDGE_CURVE('',#5268,#5265,#4818,.T.);
#6362=EDGE_CURVE('',#5263,#5268,#258,.T.);
#6363=EDGE_CURVE('',#5268,#5264,#2684,.T.);
#6364=EDGE_CURVE('',#5269,#5270,#2685,.T.);
#6365=EDGE_CURVE('',#5269,#5271,#2686,.T.);
#6366=EDGE_CURVE('',#5272,#5271,#2687,.T.);
#6367=EDGE_CURVE('',#5270,#5272,#2688,.T.);
#6368=EDGE_CURVE('',#5273,#5269,#2689,.T.);
#6369=EDGE_CURVE('',#5273,#5274,#2690,.T.);
#6370=EDGE_CURVE('',#5271,#5274,#2691,.T.);
#6371=EDGE_CURVE('',#5275,#5273,#2692,.T.);
#6372=EDGE_CURVE('',#5276,#5275,#2693,.T.);
#6373=EDGE_CURVE('',#5274,#5276,#2694,.T.);
#6374=EDGE_CURVE('',#5277,#5277,#4819,.T.);
#6375=EDGE_CURVE('',#5276,#5272,#4820,.T.);
#6376=EDGE_CURVE('',#5275,#5270,#4821,.T.);
#6377=EDGE_CURVE('',#5278,#5278,#4822,.T.);
#6378=EDGE_CURVE('',#5279,#5279,#4823,.T.);
#6379=EDGE_CURVE('',#5280,#5280,#4824,.T.);
#6380=EDGE_CURVE('',#5281,#5281,#4825,.T.);
#6381=EDGE_CURVE('',#5278,#5280,#2695,.T.);
#6382=EDGE_CURVE('',#5281,#5282,#2696,.T.);
#6383=EDGE_CURVE('',#5282,#5282,#4826,.T.);
#6384=EDGE_CURVE('',#5277,#5279,#2697,.T.);
#6385=EDGE_CURVE('',#5283,#5284,#2698,.T.);
#6386=EDGE_CURVE('',#5283,#5284,#4827,.T.);
#6387=EDGE_CURVE('',#5285,#5283,#259,.T.);
#6388=EDGE_CURVE('',#5286,#5285,#4828,.T.);
#6389=EDGE_CURVE('',#5286,#5287,#2699,.T.);
#6390=EDGE_CURVE('',#5288,#5287,#260,.T.);
#6391=EDGE_CURVE('',#5287,#5288,#261,.T.);
#6392=EDGE_CURVE('',#5289,#5286,#4829,.T.);
#6393=EDGE_CURVE('',#5284,#5289,#262,.T.);
#6394=EDGE_CURVE('',#5289,#5285,#2700,.T.);
#6395=EDGE_CURVE('',#5290,#5290,#4830,.T.);
#6396=EDGE_CURVE('',#5290,#5291,#2701,.T.);
#6397=EDGE_CURVE('',#5291,#5291,#4831,.T.);
#6398=EDGE_CURVE('',#5292,#5292,#4832,.T.);
#6399=EDGE_CURVE('',#5292,#5293,#2702,.T.);
#6400=EDGE_CURVE('',#5293,#5293,#4833,.T.);
#6401=EDGE_CURVE('',#5294,#5295,#2703,.T.);
#6402=EDGE_CURVE('',#5294,#5295,#4834,.T.);
#6403=EDGE_CURVE('',#5296,#5294,#263,.T.);
#6404=EDGE_CURVE('',#5297,#5296,#4835,.T.);
#6405=EDGE_CURVE('',#5297,#5298,#2704,.T.);
#6406=EDGE_CURVE('',#5299,#5298,#264,.T.);
#6407=EDGE_CURVE('',#5298,#5299,#265,.T.);
#6408=EDGE_CURVE('',#5300,#5297,#4836,.T.);
#6409=EDGE_CURVE('',#5295,#5300,#266,.T.);
#6410=EDGE_CURVE('',#5300,#5296,#2705,.T.);
#6411=EDGE_CURVE('',#5301,#5301,#4837,.T.);
#6412=EDGE_CURVE('',#5301,#5302,#2706,.T.);
#6413=EDGE_CURVE('',#5302,#5302,#4838,.T.);
#6414=EDGE_CURVE('',#5303,#5303,#4839,.T.);
#6415=EDGE_CURVE('',#5303,#5304,#2707,.T.);
#6416=EDGE_CURVE('',#5304,#5304,#4840,.T.);
#6417=EDGE_CURVE('',#5305,#5305,#4841,.T.);
#6418=EDGE_CURVE('',#5305,#5306,#2708,.T.);
#6419=EDGE_CURVE('',#5306,#5306,#4842,.T.);
#6420=EDGE_CURVE('',#5307,#5307,#4843,.T.);
#6421=EDGE_CURVE('',#5307,#5308,#2709,.T.);
#6422=EDGE_CURVE('',#5308,#5308,#4844,.T.);
#6423=EDGE_CURVE('',#5309,#5310,#2710,.T.);
#6424=EDGE_CURVE('',#5309,#5311,#2711,.T.);
#6425=EDGE_CURVE('',#5311,#5312,#2712,.T.);
#6426=EDGE_CURVE('',#5310,#5312,#2713,.T.);
#6427=EDGE_CURVE('',#5313,#5309,#2714,.T.);
#6428=EDGE_CURVE('',#5313,#5314,#2715,.T.);
#6429=EDGE_CURVE('',#5314,#5311,#2716,.T.);
#6430=EDGE_CURVE('',#5315,#5313,#2717,.T.);
#6431=EDGE_CURVE('',#5315,#5316,#2718,.T.);
#6432=EDGE_CURVE('',#5316,#5314,#2719,.T.);
#6433=EDGE_CURVE('',#5317,#5315,#2720,.T.);
#6434=EDGE_CURVE('',#5317,#5318,#2721,.T.);
#6435=EDGE_CURVE('',#5318,#5316,#2722,.T.);
#6436=EDGE_CURVE('',#5319,#5317,#2723,.T.);
#6437=EDGE_CURVE('',#5319,#5320,#2724,.T.);
#6438=EDGE_CURVE('',#5320,#5318,#2725,.T.);
#6439=EDGE_CURVE('',#5310,#5319,#2726,.T.);
#6440=EDGE_CURVE('',#5312,#5320,#2727,.T.);
#6441=EDGE_CURVE('',#5321,#5321,#4845,.T.);
#6442=EDGE_CURVE('',#5322,#5322,#4846,.T.);
#6443=EDGE_CURVE('',#5322,#5321,#2728,.T.);
#6444=EDGE_CURVE('',#5323,#5323,#4847,.F.);
#6445=EDGE_CURVE('',#5323,#5322,#2729,.T.);
#6446=EDGE_CURVE('',#5324,#5324,#4848,.T.);
#6447=EDGE_CURVE('',#5324,#5323,#2730,.T.);
#6448=EDGE_CURVE('',#5325,#5326,#267,.T.);
#6449=EDGE_CURVE('',#5326,#5325,#268,.T.);
#6450=EDGE_CURVE('',#5326,#5327,#2731,.T.);
#6451=EDGE_CURVE('',#5327,#5327,#269,.T.);
#6452=EDGE_CURVE('',#5328,#5328,#4849,.T.);
#6453=EDGE_CURVE('',#5328,#5329,#2732,.T.);
#6454=EDGE_CURVE('',#5329,#5329,#4850,.T.);
#6455=EDGE_CURVE('',#5330,#5331,#2733,.T.);
#6456=EDGE_CURVE('',#5330,#5332,#2734,.T.);
#6457=EDGE_CURVE('',#5333,#5332,#2735,.T.);
#6458=EDGE_CURVE('',#5331,#5333,#2736,.T.);
#6459=EDGE_CURVE('',#5331,#5334,#2737,.T.);
#6460=EDGE_CURVE('',#5335,#5333,#2738,.T.);
#6461=EDGE_CURVE('',#5334,#5335,#2739,.T.);
#6462=EDGE_CURVE('',#5334,#5336,#2740,.T.);
#6463=EDGE_CURVE('',#5337,#5335,#2741,.T.);
#6464=EDGE_CURVE('',#5336,#5337,#2742,.T.);
#6465=EDGE_CURVE('',#5336,#5338,#2743,.T.);
#6466=EDGE_CURVE('',#5339,#5337,#2744,.T.);
#6467=EDGE_CURVE('',#5338,#5339,#2745,.T.);
#6468=EDGE_CURVE('',#5338,#5340,#2746,.T.);
#6469=EDGE_CURVE('',#5341,#5339,#2747,.T.);
#6470=EDGE_CURVE('',#5340,#5341,#2748,.T.);
#6471=EDGE_CURVE('',#5340,#5342,#2749,.T.);
#6472=EDGE_CURVE('',#5343,#5341,#2750,.T.);
#6473=EDGE_CURVE('',#5342,#5343,#2751,.T.);
#6474=EDGE_CURVE('',#5342,#5344,#2752,.T.);
#6475=EDGE_CURVE('',#5345,#5343,#2753,.T.);
#6476=EDGE_CURVE('',#5344,#5345,#2754,.T.);
#6477=EDGE_CURVE('',#5344,#5346,#2755,.T.);
#6478=EDGE_CURVE('',#5347,#5345,#2756,.T.);
#6479=EDGE_CURVE('',#5346,#5347,#2757,.T.);
#6480=EDGE_CURVE('',#5346,#5348,#2758,.T.);
#6481=EDGE_CURVE('',#5349,#5347,#2759,.T.);
#6482=EDGE_CURVE('',#5348,#5349,#2760,.T.);
#6483=EDGE_CURVE('',#5348,#5350,#2761,.T.);
#6484=EDGE_CURVE('',#5351,#5349,#2762,.T.);
#6485=EDGE_CURVE('',#5350,#5351,#2763,.T.);
#6486=EDGE_CURVE('',#5350,#5352,#2764,.T.);
#6487=EDGE_CURVE('',#5353,#5351,#2765,.T.);
#6488=EDGE_CURVE('',#5352,#5353,#2766,.T.);
#6489=EDGE_CURVE('',#5352,#5354,#2767,.T.);
#6490=EDGE_CURVE('',#5355,#5353,#2768,.T.);
#6491=EDGE_CURVE('',#5354,#5355,#2769,.T.);
#6492=EDGE_CURVE('',#5354,#5356,#2770,.T.);
#6493=EDGE_CURVE('',#5357,#5355,#2771,.T.);
#6494=EDGE_CURVE('',#5356,#5357,#2772,.T.);
#6495=EDGE_CURVE('',#5356,#5358,#2773,.T.);
#6496=EDGE_CURVE('',#5359,#5357,#2774,.T.);
#6497=EDGE_CURVE('',#5358,#5359,#2775,.T.);
#6498=EDGE_CURVE('',#5358,#5360,#2776,.T.);
#6499=EDGE_CURVE('',#5361,#5359,#2777,.T.);
#6500=EDGE_CURVE('',#5360,#5361,#2778,.T.);
#6501=EDGE_CURVE('',#5360,#5362,#2779,.T.);
#6502=EDGE_CURVE('',#5363,#5361,#2780,.T.);
#6503=EDGE_CURVE('',#5362,#5363,#2781,.T.);
#6504=EDGE_CURVE('',#5362,#5364,#2782,.T.);
#6505=EDGE_CURVE('',#5365,#5363,#2783,.T.);
#6506=EDGE_CURVE('',#5364,#5365,#2784,.T.);
#6507=EDGE_CURVE('',#5364,#5330,#2785,.T.);
#6508=EDGE_CURVE('',#5332,#5365,#2786,.T.);
#6509=EDGE_CURVE('',#5332,#5333,#4851,.T.);
#6510=EDGE_CURVE('',#5333,#5335,#4852,.T.);
#6511=EDGE_CURVE('',#5335,#5337,#4853,.T.);
#6512=EDGE_CURVE('',#5337,#5339,#4854,.T.);
#6513=EDGE_CURVE('',#5339,#5341,#4855,.T.);
#6514=EDGE_CURVE('',#5341,#5343,#4856,.T.);
#6515=EDGE_CURVE('',#5343,#5345,#4857,.T.);
#6516=EDGE_CURVE('',#5345,#5347,#4858,.T.);
#6517=EDGE_CURVE('',#5347,#5366,#4859,.T.);
#6518=EDGE_CURVE('',#5366,#5367,#2787,.T.);
#6519=EDGE_CURVE('',#5367,#5368,#2788,.T.);
#6520=EDGE_CURVE('',#5368,#5369,#2789,.T.);
#6521=EDGE_CURVE('',#5369,#5370,#2790,.T.);
#6522=EDGE_CURVE('',#5370,#5371,#2791,.T.);
#6523=EDGE_CURVE('',#5371,#5372,#2792,.T.);
#6524=EDGE_CURVE('',#5372,#5373,#2793,.T.);
#6525=EDGE_CURVE('',#5373,#5374,#2794,.T.);
#6526=EDGE_CURVE('',#5374,#5375,#2795,.T.);
#6527=EDGE_CURVE('',#5375,#5376,#2796,.T.);
#6528=EDGE_CURVE('',#5376,#5377,#4860,.T.);
#6529=EDGE_CURVE('',#5377,#5378,#2797,.T.);
#6530=EDGE_CURVE('',#5378,#5379,#2798,.T.);
#6531=EDGE_CURVE('',#5379,#5380,#2799,.T.);
#6532=EDGE_CURVE('',#5380,#5381,#2800,.T.);
#6533=EDGE_CURVE('',#5381,#5382,#2801,.T.);
#6534=EDGE_CURVE('',#5382,#5383,#2802,.T.);
#6535=EDGE_CURVE('',#5383,#5384,#2803,.T.);
#6536=EDGE_CURVE('',#5384,#5385,#2804,.T.);
#6537=EDGE_CURVE('',#5385,#5386,#2805,.T.);
#6538=EDGE_CURVE('',#5386,#5387,#2806,.T.);
#6539=EDGE_CURVE('',#5387,#5388,#4861,.T.);
#6540=EDGE_CURVE('',#5388,#5332,#4862,.T.);
#6541=EDGE_CURVE('',#5389,#5390,#2807,.T.);
#6542=EDGE_CURVE('',#5389,#5377,#2808,.T.);
#6543=EDGE_CURVE('',#5391,#5377,#2809,.T.);
#6544=EDGE_CURVE('',#5390,#5391,#2810,.T.);
#6545=EDGE_CURVE('',#5390,#5392,#2811,.T.);
#6546=EDGE_CURVE('',#5393,#5391,#2812,.T.);
#6547=EDGE_CURVE('',#5392,#5393,#2813,.T.);
#6548=EDGE_CURVE('',#5392,#5394,#2814,.T.);
#6549=EDGE_CURVE('',#5395,#5393,#2815,.T.);
#6550=EDGE_CURVE('',#5394,#5395,#2816,.T.);
#6551=EDGE_CURVE('',#5394,#5396,#2817,.T.);
#6552=EDGE_CURVE('',#5397,#5395,#2818,.T.);
#6553=EDGE_CURVE('',#5396,#5397,#2819,.T.);
#6554=EDGE_CURVE('',#5396,#5398,#2820,.T.);
#6555=EDGE_CURVE('',#5399,#5397,#2821,.T.);
#6556=EDGE_CURVE('',#5398,#5399,#2822,.T.);
#6557=EDGE_CURVE('',#5398,#5400,#2823,.T.);
#6558=EDGE_CURVE('',#5401,#5399,#2824,.T.);
#6559=EDGE_CURVE('',#5400,#5401,#2825,.T.);
#6560=EDGE_CURVE('',#5400,#5402,#2826,.T.);
#6561=EDGE_CURVE('',#5403,#5401,#2827,.T.);
#6562=EDGE_CURVE('',#5402,#5403,#2828,.T.);
#6563=EDGE_CURVE('',#5402,#5404,#2829,.T.);
#6564=EDGE_CURVE('',#5387,#5403,#2830,.T.);
#6565=EDGE_CURVE('',#5404,#5387,#2831,.T.);
#6566=EDGE_CURVE('',#5404,#5405,#2832,.T.);
#6567=EDGE_CURVE('',#5405,#5386,#2833,.T.);
#6568=EDGE_CURVE('',#5405,#5406,#2834,.T.);
#6569=EDGE_CURVE('',#5406,#5385,#2835,.T.);
#6570=EDGE_CURVE('',#5406,#5407,#2836,.T.);
#6571=EDGE_CURVE('',#5407,#5384,#2837,.T.);
#6572=EDGE_CURVE('',#5407,#5408,#2838,.T.);
#6573=EDGE_CURVE('',#5408,#5383,#2839,.T.);
#6574=EDGE_CURVE('',#5408,#5409,#2840,.T.);
#6575=EDGE_CURVE('',#5409,#5382,#2841,.T.);
#6576=EDGE_CURVE('',#5409,#5410,#2842,.T.);
#6577=EDGE_CURVE('',#5410,#5381,#2843,.T.);
#6578=EDGE_CURVE('',#5410,#5411,#2844,.T.);
#6579=EDGE_CURVE('',#5411,#5380,#2845,.T.);
#6580=EDGE_CURVE('',#5411,#5412,#2846,.T.);
#6581=EDGE_CURVE('',#5412,#5379,#2847,.T.);
#6582=EDGE_CURVE('',#5412,#5413,#2848,.T.);
#6583=EDGE_CURVE('',#5413,#5378,#2849,.T.);
#6584=EDGE_CURVE('',#5413,#5389,#2850,.T.);
#6585=EDGE_CURVE('',#5377,#5391,#4863,.T.);
#6586=EDGE_CURVE('',#5391,#5393,#4864,.T.);
#6587=EDGE_CURVE('',#5393,#5395,#4865,.T.);
#6588=EDGE_CURVE('',#5395,#5397,#4866,.T.);
#6589=EDGE_CURVE('',#5397,#5399,#4867,.T.);
#6590=EDGE_CURVE('',#5399,#5401,#4868,.T.);
#6591=EDGE_CURVE('',#5401,#5403,#4869,.T.);
#6592=EDGE_CURVE('',#5403,#5387,#4870,.T.);
#6593=EDGE_CURVE('',#5414,#5415,#2851,.T.);
#6594=EDGE_CURVE('',#5414,#5366,#2852,.T.);
#6595=EDGE_CURVE('',#5416,#5366,#2853,.T.);
#6596=EDGE_CURVE('',#5415,#5416,#2854,.T.);
#6597=EDGE_CURVE('',#5415,#5417,#2855,.T.);
#6598=EDGE_CURVE('',#5418,#5416,#2856,.T.);
#6599=EDGE_CURVE('',#5417,#5418,#2857,.T.);
#6600=EDGE_CURVE('',#5417,#5419,#2858,.T.);
#6601=EDGE_CURVE('',#5420,#5418,#2859,.T.);
#6602=EDGE_CURVE('',#5419,#5420,#2860,.T.);
#6603=EDGE_CURVE('',#5419,#5421,#2861,.T.);
#6604=EDGE_CURVE('',#5422,#5420,#2862,.T.);
#6605=EDGE_CURVE('',#5421,#5422,#2863,.T.);
#6606=EDGE_CURVE('',#5421,#5423,#2864,.T.);
#6607=EDGE_CURVE('',#5424,#5422,#2865,.T.);
#6608=EDGE_CURVE('',#5423,#5424,#2866,.T.);
#6609=EDGE_CURVE('',#5423,#5425,#2867,.T.);
#6610=EDGE_CURVE('',#5426,#5424,#2868,.T.);
#6611=EDGE_CURVE('',#5425,#5426,#2869,.T.);
#6612=EDGE_CURVE('',#5425,#5427,#2870,.T.);
#6613=EDGE_CURVE('',#5428,#5426,#2871,.T.);
#6614=EDGE_CURVE('',#5427,#5428,#2872,.T.);
#6615=EDGE_CURVE('',#5427,#5429,#2873,.T.);
#6616=EDGE_CURVE('',#5376,#5428,#2874,.T.);
#6617=EDGE_CURVE('',#5429,#5376,#2875,.T.);
#6618=EDGE_CURVE('',#5429,#5430,#2876,.T.);
#6619=EDGE_CURVE('',#5430,#5375,#2877,.T.);
#6620=EDGE_CURVE('',#5430,#5431,#2878,.T.);
#6621=EDGE_CURVE('',#5431,#5374,#2879,.T.);
#6622=EDGE_CURVE('',#5431,#5432,#2880,.T.);
#6623=EDGE_CURVE('',#5432,#5373,#2881,.T.);
#6624=EDGE_CURVE('',#5432,#5433,#2882,.T.);
#6625=EDGE_CURVE('',#5433,#5372,#2883,.T.);
#6626=EDGE_CURVE('',#5433,#5434,#2884,.T.);
#6627=EDGE_CURVE('',#5434,#5371,#2885,.T.);
#6628=EDGE_CURVE('',#5434,#5435,#2886,.T.);
#6629=EDGE_CURVE('',#5435,#5370,#2887,.T.);
#6630=EDGE_CURVE('',#5435,#5436,#2888,.T.);
#6631=EDGE_CURVE('',#5436,#5369,#2889,.T.);
#6632=EDGE_CURVE('',#5436,#5437,#2890,.T.);
#6633=EDGE_CURVE('',#5437,#5368,#2891,.T.);
#6634=EDGE_CURVE('',#5437,#5438,#2892,.T.);
#6635=EDGE_CURVE('',#5438,#5367,#2893,.T.);
#6636=EDGE_CURVE('',#5438,#5414,#2894,.T.);
#6637=EDGE_CURVE('',#5366,#5416,#4871,.T.);
#6638=EDGE_CURVE('',#5416,#5418,#4872,.T.);
#6639=EDGE_CURVE('',#5418,#5420,#4873,.T.);
#6640=EDGE_CURVE('',#5420,#5422,#4874,.T.);
#6641=EDGE_CURVE('',#5422,#5424,#4875,.T.);
#6642=EDGE_CURVE('',#5424,#5426,#4876,.T.);
#6643=EDGE_CURVE('',#5426,#5428,#4877,.T.);
#6644=EDGE_CURVE('',#5428,#5376,#4878,.T.);
#6645=EDGE_CURVE('',#5439,#5439,#4879,.T.);
#6646=EDGE_CURVE('',#5439,#5388,#2895,.T.);
#6647=EDGE_CURVE('',#5440,#5441,#270,.T.);
#6648=EDGE_CURVE('',#5441,#5440,#271,.T.);
#6649=EDGE_CURVE('',#5441,#5442,#2896,.T.);
#6650=EDGE_CURVE('',#5443,#5442,#272,.T.);
#6651=EDGE_CURVE('',#5442,#5443,#273,.T.);
#6652=EDGE_CURVE('',#5444,#5444,#4880,.T.);
#6653=EDGE_CURVE('',#5444,#5445,#2897,.T.);
#6654=EDGE_CURVE('',#5445,#5445,#4881,.T.);
#6655=EDGE_CURVE('',#5446,#5447,#2898,.T.);
#6656=EDGE_CURVE('',#5447,#5448,#2899,.T.);
#6657=EDGE_CURVE('',#5449,#5448,#2900,.T.);
#6658=EDGE_CURVE('',#5446,#5449,#2901,.T.);
#6659=EDGE_CURVE('',#5450,#5446,#2902,.T.);
#6660=EDGE_CURVE('',#5451,#5449,#2903,.T.);
#6661=EDGE_CURVE('',#5450,#5451,#2904,.T.);
#6662=EDGE_CURVE('',#5452,#5450,#2905,.T.);
#6663=EDGE_CURVE('',#5453,#5451,#2906,.T.);
#6664=EDGE_CURVE('',#5452,#5453,#2907,.T.);
#6665=EDGE_CURVE('',#5454,#5452,#2908,.T.);
#6666=EDGE_CURVE('',#5455,#5453,#2909,.T.);
#6667=EDGE_CURVE('',#5454,#5455,#2910,.T.);
#6668=EDGE_CURVE('',#5456,#5454,#2911,.T.);
#6669=EDGE_CURVE('',#5457,#5455,#2912,.T.);
#6670=EDGE_CURVE('',#5456,#5457,#2913,.T.);
#6671=EDGE_CURVE('',#5458,#5456,#2914,.T.);
#6672=EDGE_CURVE('',#5459,#5457,#2915,.T.);
#6673=EDGE_CURVE('',#5458,#5459,#2916,.T.);
#6674=EDGE_CURVE('',#5460,#5458,#2917,.T.);
#6675=EDGE_CURVE('',#5461,#5459,#2918,.T.);
#6676=EDGE_CURVE('',#5460,#5461,#2919,.T.);
#6677=EDGE_CURVE('',#5462,#5460,#2920,.T.);
#6678=EDGE_CURVE('',#5463,#5461,#2921,.T.);
#6679=EDGE_CURVE('',#5462,#5463,#2922,.T.);
#6680=EDGE_CURVE('',#5464,#5462,#2923,.T.);
#6681=EDGE_CURVE('',#5465,#5463,#2924,.T.);
#6682=EDGE_CURVE('',#5464,#5465,#2925,.T.);
#6683=EDGE_CURVE('',#5466,#5464,#2926,.T.);
#6684=EDGE_CURVE('',#5467,#5465,#2927,.T.);
#6685=EDGE_CURVE('',#5466,#5467,#2928,.T.);
#6686=EDGE_CURVE('',#5468,#5466,#2929,.T.);
#6687=EDGE_CURVE('',#5469,#5467,#2930,.T.);
#6688=EDGE_CURVE('',#5468,#5469,#2931,.T.);
#6689=EDGE_CURVE('',#5470,#5468,#2932,.T.);
#6690=EDGE_CURVE('',#5471,#5469,#2933,.T.);
#6691=EDGE_CURVE('',#5470,#5471,#2934,.T.);
#6692=EDGE_CURVE('',#5472,#5470,#2935,.T.);
#6693=EDGE_CURVE('',#5473,#5471,#2936,.T.);
#6694=EDGE_CURVE('',#5472,#5473,#2937,.T.);
#6695=EDGE_CURVE('',#5474,#5472,#2938,.T.);
#6696=EDGE_CURVE('',#5475,#5473,#2939,.T.);
#6697=EDGE_CURVE('',#5474,#5475,#2940,.T.);
#6698=EDGE_CURVE('',#5476,#5474,#2941,.T.);
#6699=EDGE_CURVE('',#5477,#5475,#2942,.T.);
#6700=EDGE_CURVE('',#5476,#5477,#2943,.T.);
#6701=EDGE_CURVE('',#5478,#5476,#2944,.T.);
#6702=EDGE_CURVE('',#5479,#5477,#2945,.T.);
#6703=EDGE_CURVE('',#5478,#5479,#2946,.T.);
#6704=EDGE_CURVE('',#5480,#5478,#2947,.T.);
#6705=EDGE_CURVE('',#5481,#5479,#2948,.T.);
#6706=EDGE_CURVE('',#5480,#5481,#2949,.T.);
#6707=EDGE_CURVE('',#5447,#5480,#2950,.T.);
#6708=EDGE_CURVE('',#5448,#5481,#2951,.T.);
#6709=EDGE_CURVE('',#5481,#5479,#4882,.T.);
#6710=EDGE_CURVE('',#5479,#5477,#4883,.T.);
#6711=EDGE_CURVE('',#5477,#5475,#4884,.T.);
#6712=EDGE_CURVE('',#5475,#5473,#4885,.T.);
#6713=EDGE_CURVE('',#5473,#5471,#4886,.T.);
#6714=EDGE_CURVE('',#5471,#5469,#4887,.T.);
#6715=EDGE_CURVE('',#5482,#5481,#4888,.T.);
#6716=EDGE_CURVE('',#5483,#5482,#4889,.T.);
#6717=EDGE_CURVE('',#5483,#5484,#2952,.T.);
#6718=EDGE_CURVE('',#5484,#5485,#2953,.T.);
#6719=EDGE_CURVE('',#5485,#5486,#2954,.T.);
#6720=EDGE_CURVE('',#5486,#5487,#2955,.T.);
#6721=EDGE_CURVE('',#5487,#5488,#2956,.T.);
#6722=EDGE_CURVE('',#5488,#5489,#2957,.T.);
#6723=EDGE_CURVE('',#5489,#5490,#2958,.T.);
#6724=EDGE_CURVE('',#5490,#5491,#2959,.T.);
#6725=EDGE_CURVE('',#5491,#5492,#2960,.T.);
#6726=EDGE_CURVE('',#5492,#5493,#2961,.T.);
#6727=EDGE_CURVE('',#5494,#5493,#4890,.T.);
#6728=EDGE_CURVE('',#5494,#5495,#2962,.T.);
#6729=EDGE_CURVE('',#5495,#5496,#2963,.T.);
#6730=EDGE_CURVE('',#5496,#5497,#2964,.T.);
#6731=EDGE_CURVE('',#5497,#5498,#2965,.T.);
#6732=EDGE_CURVE('',#5498,#5499,#2966,.T.);
#6733=EDGE_CURVE('',#5499,#5500,#2967,.T.);
#6734=EDGE_CURVE('',#5500,#5501,#2968,.T.);
#6735=EDGE_CURVE('',#5501,#5502,#2969,.T.);
#6736=EDGE_CURVE('',#5502,#5503,#2970,.T.);
#6737=EDGE_CURVE('',#5503,#5504,#2971,.T.);
#6738=EDGE_CURVE('',#5465,#5504,#4891,.T.);
#6739=EDGE_CURVE('',#5467,#5465,#4892,.T.);
#6740=EDGE_CURVE('',#5469,#5467,#4893,.T.);
#6741=EDGE_CURVE('',#5505,#5506,#2972,.T.);
#6742=EDGE_CURVE('',#5506,#5492,#2973,.T.);
#6743=EDGE_CURVE('',#5505,#5491,#2974,.T.);
#6744=EDGE_CURVE('',#5507,#5505,#2975,.T.);
#6745=EDGE_CURVE('',#5507,#5490,#2976,.T.);
#6746=EDGE_CURVE('',#5508,#5507,#2977,.T.);
#6747=EDGE_CURVE('',#5508,#5489,#2978,.T.);
#6748=EDGE_CURVE('',#5509,#5508,#2979,.T.);
#6749=EDGE_CURVE('',#5509,#5488,#2980,.T.);
#6750=EDGE_CURVE('',#5510,#5509,#2981,.T.);
#6751=EDGE_CURVE('',#5510,#5487,#2982,.T.);
#6752=EDGE_CURVE('',#5511,#5510,#2983,.T.);
#6753=EDGE_CURVE('',#5511,#5486,#2984,.T.);
#6754=EDGE_CURVE('',#5512,#5511,#2985,.T.);
#6755=EDGE_CURVE('',#5512,#5485,#2986,.T.);
#6756=EDGE_CURVE('',#5513,#5512,#2987,.T.);
#6757=EDGE_CURVE('',#5513,#5484,#2988,.T.);
#6758=EDGE_CURVE('',#5514,#5513,#2989,.T.);
#6759=EDGE_CURVE('',#5514,#5483,#2990,.T.);
#6760=EDGE_CURVE('',#5515,#5514,#2991,.T.);
#6761=EDGE_CURVE('',#5516,#5483,#2992,.T.);
#6762=EDGE_CURVE('',#5515,#5516,#2993,.T.);
#6763=EDGE_CURVE('',#5517,#5515,#2994,.T.);
#6764=EDGE_CURVE('',#5518,#5516,#2995,.T.);
#6765=EDGE_CURVE('',#5517,#5518,#2996,.T.);
#6766=EDGE_CURVE('',#5519,#5517,#2997,.T.);
#6767=EDGE_CURVE('',#5520,#5518,#2998,.T.);
#6768=EDGE_CURVE('',#5519,#5520,#2999,.T.);
#6769=EDGE_CURVE('',#5521,#5519,#3000,.T.);
#6770=EDGE_CURVE('',#5522,#5520,#3001,.T.);
#6771=EDGE_CURVE('',#5521,#5522,#3002,.T.);
#6772=EDGE_CURVE('',#5523,#5521,#3003,.T.);
#6773=EDGE_CURVE('',#5524,#5522,#3004,.T.);
#6774=EDGE_CURVE('',#5523,#5524,#3005,.T.);
#6775=EDGE_CURVE('',#5525,#5523,#3006,.T.);
#6776=EDGE_CURVE('',#5526,#5524,#3007,.T.);
#6777=EDGE_CURVE('',#5525,#5526,#3008,.T.);
#6778=EDGE_CURVE('',#5527,#5525,#3009,.T.);
#6779=EDGE_CURVE('',#5528,#5526,#3010,.T.);
#6780=EDGE_CURVE('',#5527,#5528,#3011,.T.);
#6781=EDGE_CURVE('',#5529,#5527,#3012,.T.);
#6782=EDGE_CURVE('',#5493,#5528,#3013,.T.);
#6783=EDGE_CURVE('',#5529,#5493,#3014,.T.);
#6784=EDGE_CURVE('',#5506,#5529,#3015,.T.);
#6785=EDGE_CURVE('',#5493,#5528,#4894,.T.);
#6786=EDGE_CURVE('',#5528,#5526,#4895,.T.);
#6787=EDGE_CURVE('',#5526,#5524,#4896,.T.);
#6788=EDGE_CURVE('',#5524,#5522,#4897,.T.);
#6789=EDGE_CURVE('',#5522,#5520,#4898,.T.);
#6790=EDGE_CURVE('',#5520,#5518,#4899,.T.);
#6791=EDGE_CURVE('',#5516,#5483,#4900,.T.);
#6792=EDGE_CURVE('',#5518,#5516,#4901,.T.);
#6793=EDGE_CURVE('',#5530,#5531,#3016,.T.);
#6794=EDGE_CURVE('',#5531,#5503,#3017,.T.);
#6795=EDGE_CURVE('',#5530,#5502,#3018,.T.);
#6796=EDGE_CURVE('',#5532,#5530,#3019,.T.);
#6797=EDGE_CURVE('',#5532,#5501,#3020,.T.);
#6798=EDGE_CURVE('',#5533,#5532,#3021,.T.);
#6799=EDGE_CURVE('',#5533,#5500,#3022,.T.);
#6800=EDGE_CURVE('',#5534,#5533,#3023,.T.);
#6801=EDGE_CURVE('',#5534,#5499,#3024,.T.);
#6802=EDGE_CURVE('',#5535,#5534,#3025,.T.);
#6803=EDGE_CURVE('',#5535,#5498,#3026,.T.);
#6804=EDGE_CURVE('',#5536,#5535,#3027,.T.);
#6805=EDGE_CURVE('',#5536,#5497,#3028,.T.);
#6806=EDGE_CURVE('',#5537,#5536,#3029,.T.);
#6807=EDGE_CURVE('',#5537,#5496,#3030,.T.);
#6808=EDGE_CURVE('',#5538,#5537,#3031,.T.);
#6809=EDGE_CURVE('',#5538,#5495,#3032,.T.);
#6810=EDGE_CURVE('',#5539,#5538,#3033,.T.);
#6811=EDGE_CURVE('',#5539,#5494,#3034,.T.);
#6812=EDGE_CURVE('',#5540,#5539,#3035,.T.);
#6813=EDGE_CURVE('',#5541,#5494,#3036,.T.);
#6814=EDGE_CURVE('',#5540,#5541,#3037,.T.);
#6815=EDGE_CURVE('',#5542,#5540,#3038,.T.);
#6816=EDGE_CURVE('',#5543,#5541,#3039,.T.);
#6817=EDGE_CURVE('',#5542,#5543,#3040,.T.);
#6818=EDGE_CURVE('',#5544,#5542,#3041,.T.);
#6819=EDGE_CURVE('',#5545,#5543,#3042,.T.);
#6820=EDGE_CURVE('',#5544,#5545,#3043,.T.);
#6821=EDGE_CURVE('',#5546,#5544,#3044,.T.);
#6822=EDGE_CURVE('',#5547,#5545,#3045,.T.);
#6823=EDGE_CURVE('',#5546,#5547,#3046,.T.);
#6824=EDGE_CURVE('',#5548,#5546,#3047,.T.);
#6825=EDGE_CURVE('',#5549,#5547,#3048,.T.);
#6826=EDGE_CURVE('',#5548,#5549,#3049,.T.);
#6827=EDGE_CURVE('',#5550,#5548,#3050,.T.);
#6828=EDGE_CURVE('',#5551,#5549,#3051,.T.);
#6829=EDGE_CURVE('',#5550,#5551,#3052,.T.);
#6830=EDGE_CURVE('',#5552,#5550,#3053,.T.);
#6831=EDGE_CURVE('',#5553,#5551,#3054,.T.);
#6832=EDGE_CURVE('',#5552,#5553,#3055,.T.);
#6833=EDGE_CURVE('',#5554,#5552,#3056,.T.);
#6834=EDGE_CURVE('',#5504,#5553,#3057,.T.);
#6835=EDGE_CURVE('',#5554,#5504,#3058,.T.);
#6836=EDGE_CURVE('',#5531,#5554,#3059,.T.);
#6837=EDGE_CURVE('',#5504,#5553,#4902,.T.);
#6838=EDGE_CURVE('',#5553,#5551,#4903,.T.);
#6839=EDGE_CURVE('',#5551,#5549,#4904,.T.);
#6840=EDGE_CURVE('',#5549,#5547,#4905,.T.);
#6841=EDGE_CURVE('',#5547,#5545,#4906,.T.);
#6842=EDGE_CURVE('',#5545,#5543,#4907,.T.);
#6843=EDGE_CURVE('',#5541,#5494,#4908,.T.);
#6844=EDGE_CURVE('',#5543,#5541,#4909,.T.);
#6845=EDGE_CURVE('',#5555,#5555,#4910,.T.);
#6846=EDGE_CURVE('',#5555,#5482,#3060,.T.);
#6847=EDGE_CURVE('',#5556,#5557,#3061,.T.);
#6848=EDGE_CURVE('',#5558,#5556,#3062,.T.);
#6849=EDGE_CURVE('',#5559,#5558,#3063,.T.);
#6850=EDGE_CURVE('',#5560,#5559,#3064,.T.);
#6851=EDGE_CURVE('',#5561,#5560,#3065,.T.);
#6852=EDGE_CURVE('',#5562,#5561,#3066,.T.);
#6853=EDGE_CURVE('',#5563,#5562,#3067,.T.);
#6854=EDGE_CURVE('',#5564,#5563,#3068,.T.);
#6855=EDGE_CURVE('',#5564,#5565,#4911,.T.);
#6856=EDGE_CURVE('',#5566,#5565,#3069,.T.);
#6857=EDGE_CURVE('',#5567,#5566,#3070,.T.);
#6858=EDGE_CURVE('',#5568,#5567,#3071,.T.);
#6859=EDGE_CURVE('',#5569,#5568,#3072,.T.);
#6860=EDGE_CURVE('',#5570,#5569,#3073,.T.);
#6861=EDGE_CURVE('',#5571,#5570,#3074,.T.);
#6862=EDGE_CURVE('',#5572,#5571,#3075,.T.);
#6863=EDGE_CURVE('',#5573,#5572,#3076,.T.);
#6864=EDGE_CURVE('',#5573,#5574,#4912,.T.);
#6865=EDGE_CURVE('',#5575,#5574,#3077,.T.);
#6866=EDGE_CURVE('',#5576,#5575,#3078,.T.);
#6867=EDGE_CURVE('',#5577,#5576,#3079,.T.);
#6868=EDGE_CURVE('',#5578,#5577,#3080,.T.);
#6869=EDGE_CURVE('',#5579,#5578,#3081,.T.);
#6870=EDGE_CURVE('',#5580,#5579,#3082,.T.);
#6871=EDGE_CURVE('',#5581,#5580,#3083,.T.);
#6872=EDGE_CURVE('',#5582,#5581,#3084,.T.);
#6873=EDGE_CURVE('',#5582,#5583,#4913,.T.);
#6874=EDGE_CURVE('',#5584,#5583,#3085,.T.);
#6875=EDGE_CURVE('',#5585,#5584,#3086,.T.);
#6876=EDGE_CURVE('',#5586,#5585,#3087,.T.);
#6877=EDGE_CURVE('',#5587,#5586,#3088,.T.);
#6878=EDGE_CURVE('',#5588,#5587,#3089,.T.);
#6879=EDGE_CURVE('',#5589,#5588,#3090,.T.);
#6880=EDGE_CURVE('',#5590,#5589,#3091,.T.);
#6881=EDGE_CURVE('',#5591,#5590,#3092,.T.);
#6882=EDGE_CURVE('',#5591,#5592,#4914,.T.);
#6883=EDGE_CURVE('',#5593,#5592,#3093,.T.);
#6884=EDGE_CURVE('',#5594,#5593,#3094,.T.);
#6885=EDGE_CURVE('',#5595,#5594,#3095,.T.);
#6886=EDGE_CURVE('',#5596,#5595,#3096,.T.);
#6887=EDGE_CURVE('',#5597,#5596,#3097,.T.);
#6888=EDGE_CURVE('',#5598,#5597,#3098,.T.);
#6889=EDGE_CURVE('',#5599,#5598,#3099,.T.);
#6890=EDGE_CURVE('',#5600,#5599,#3100,.T.);
#6891=EDGE_CURVE('',#5600,#5601,#4915,.T.);
#6892=EDGE_CURVE('',#5602,#5601,#3101,.T.);
#6893=EDGE_CURVE('',#5603,#5602,#3102,.T.);
#6894=EDGE_CURVE('',#5604,#5603,#3103,.T.);
#6895=EDGE_CURVE('',#5605,#5604,#3104,.T.);
#6896=EDGE_CURVE('',#5606,#5605,#3105,.T.);
#6897=EDGE_CURVE('',#5607,#5606,#3106,.T.);
#6898=EDGE_CURVE('',#5608,#5607,#3107,.T.);
#6899=EDGE_CURVE('',#5609,#5608,#3108,.T.);
#6900=EDGE_CURVE('',#5609,#5557,#4916,.T.);
#6901=EDGE_CURVE('',#5610,#5600,#3109,.T.);
#6902=EDGE_CURVE('',#5611,#5610,#4917,.T.);
#6903=EDGE_CURVE('',#5601,#5611,#3110,.T.);
#6904=EDGE_CURVE('',#5612,#5564,#3111,.T.);
#6905=EDGE_CURVE('',#5613,#5612,#4918,.T.);
#6906=EDGE_CURVE('',#5565,#5613,#3112,.T.);
#6907=EDGE_CURVE('',#5614,#5582,#3113,.T.);
#6908=EDGE_CURVE('',#5615,#5614,#4919,.T.);
#6909=EDGE_CURVE('',#5583,#5615,#3114,.T.);
#6910=EDGE_CURVE('',#5592,#5616,#3115,.T.);
#6911=EDGE_CURVE('',#5617,#5591,#3116,.T.);
#6912=EDGE_CURVE('',#5616,#5617,#4920,.T.);
#6913=EDGE_CURVE('',#5574,#5618,#3117,.T.);
#6914=EDGE_CURVE('',#5619,#5573,#3118,.T.);
#6915=EDGE_CURVE('',#5618,#5619,#4921,.T.);
#6916=EDGE_CURVE('',#5557,#5620,#3119,.T.);
#6917=EDGE_CURVE('',#5621,#5609,#3120,.T.);
#6918=EDGE_CURVE('',#5620,#5621,#4922,.T.);
#6919=EDGE_CURVE('',#5620,#5622,#3121,.T.);
#6920=EDGE_CURVE('',#5623,#5621,#3122,.T.);
#6921=EDGE_CURVE('',#5624,#5623,#3123,.T.);
#6922=EDGE_CURVE('',#5625,#5624,#3124,.T.);
#6923=EDGE_CURVE('',#5626,#5625,#3125,.T.);
#6924=EDGE_CURVE('',#5627,#5626,#3126,.T.);
#6925=EDGE_CURVE('',#5628,#5627,#3127,.T.);
#6926=EDGE_CURVE('',#5629,#5628,#3128,.T.);
#6927=EDGE_CURVE('',#5611,#5629,#3129,.T.);
#6928=EDGE_CURVE('',#5630,#5610,#3130,.T.);
#6929=EDGE_CURVE('',#5631,#5630,#3131,.T.);
#6930=EDGE_CURVE('',#5632,#5631,#3132,.T.);
#6931=EDGE_CURVE('',#5633,#5632,#3133,.T.);
#6932=EDGE_CURVE('',#5634,#5633,#3134,.T.);
#6933=EDGE_CURVE('',#5635,#5634,#3135,.T.);
#6934=EDGE_CURVE('',#5636,#5635,#3136,.T.);
#6935=EDGE_CURVE('',#5616,#5636,#3137,.T.);
#6936=EDGE_CURVE('',#5637,#5617,#3138,.T.);
#6937=EDGE_CURVE('',#5638,#5637,#3139,.T.);
#6938=EDGE_CURVE('',#5639,#5638,#3140,.T.);
#6939=EDGE_CURVE('',#5640,#5639,#3141,.T.);
#6940=EDGE_CURVE('',#5641,#5640,#3142,.T.);
#6941=EDGE_CURVE('',#5642,#5641,#3143,.T.);
#6942=EDGE_CURVE('',#5643,#5642,#3144,.T.);
#6943=EDGE_CURVE('',#5615,#5643,#3145,.T.);
#6944=EDGE_CURVE('',#5644,#5614,#3146,.T.);
#6945=EDGE_CURVE('',#5645,#5644,#3147,.T.);
#6946=EDGE_CURVE('',#5646,#5645,#3148,.T.);
#6947=EDGE_CURVE('',#5647,#5646,#3149,.T.);
#6948=EDGE_CURVE('',#5648,#5647,#3150,.T.);
#6949=EDGE_CURVE('',#5649,#5648,#3151,.T.);
#6950=EDGE_CURVE('',#5650,#5649,#3152,.T.);
#6951=EDGE_CURVE('',#5618,#5650,#3153,.T.);
#6952=EDGE_CURVE('',#5651,#5619,#3154,.T.);
#6953=EDGE_CURVE('',#5652,#5651,#3155,.T.);
#6954=EDGE_CURVE('',#5653,#5652,#3156,.T.);
#6955=EDGE_CURVE('',#5654,#5653,#3157,.T.);
#6956=EDGE_CURVE('',#5655,#5654,#3158,.T.);
#6957=EDGE_CURVE('',#5656,#5655,#3159,.T.);
#6958=EDGE_CURVE('',#5657,#5656,#3160,.T.);
#6959=EDGE_CURVE('',#5613,#5657,#3161,.T.);
#6960=EDGE_CURVE('',#5658,#5612,#3162,.T.);
#6961=EDGE_CURVE('',#5659,#5658,#3163,.T.);
#6962=EDGE_CURVE('',#5660,#5659,#3164,.T.);
#6963=EDGE_CURVE('',#5661,#5660,#3165,.T.);
#6964=EDGE_CURVE('',#5662,#5661,#3166,.T.);
#6965=EDGE_CURVE('',#5663,#5662,#3167,.T.);
#6966=EDGE_CURVE('',#5622,#5663,#3168,.T.);
#6967=EDGE_CURVE('',#5629,#5664,#3169,.T.);
#6968=EDGE_CURVE('',#5665,#5664,#3170,.T.);
#6969=EDGE_CURVE('',#5666,#5665,#3171,.T.);
#6970=EDGE_CURVE('',#5667,#5666,#3172,.T.);
#6971=EDGE_CURVE('',#5667,#5602,#3173,.T.);
#6972=EDGE_CURVE('',#5628,#5668,#3174,.T.);
#6973=EDGE_CURVE('',#5664,#5668,#3175,.T.);
#6974=EDGE_CURVE('',#5669,#5667,#3176,.T.);
#6975=EDGE_CURVE('',#5669,#5603,#3177,.T.);
#6976=EDGE_CURVE('',#5627,#5670,#3178,.T.);
#6977=EDGE_CURVE('',#5668,#5670,#3179,.T.);
#6978=EDGE_CURVE('',#5626,#5671,#3180,.T.);
#6979=EDGE_CURVE('',#5670,#5671,#3181,.T.);
#6980=EDGE_CURVE('',#5625,#5672,#3182,.T.);
#6981=EDGE_CURVE('',#5671,#5672,#3183,.T.);
#6982=EDGE_CURVE('',#5624,#5673,#3184,.T.);
#6983=EDGE_CURVE('',#5672,#5673,#3185,.T.);
#6984=EDGE_CURVE('',#5674,#5623,#3186,.T.);
#6985=EDGE_CURVE('',#5673,#5674,#3187,.T.);
#6986=EDGE_CURVE('',#5675,#5676,#3188,.T.);
#6987=EDGE_CURVE('',#5676,#5677,#3189,.T.);
#6988=EDGE_CURVE('',#5677,#5678,#3190,.T.);
#6989=EDGE_CURVE('',#5678,#5679,#3191,.T.);
#6990=EDGE_CURVE('',#5679,#5680,#3192,.T.);
#6991=EDGE_CURVE('',#5680,#5669,#3193,.T.);
#6992=EDGE_CURVE('',#5666,#5681,#3194,.T.);
#6993=EDGE_CURVE('',#5681,#5682,#3195,.T.);
#6994=EDGE_CURVE('',#5682,#5683,#3196,.T.);
#6995=EDGE_CURVE('',#5683,#5684,#3197,.T.);
#6996=EDGE_CURVE('',#5684,#5685,#3198,.T.);
#6997=EDGE_CURVE('',#5685,#5675,#3199,.T.);
#6998=EDGE_CURVE('',#5677,#5607,#3200,.T.);
#6999=EDGE_CURVE('',#5608,#5676,#3201,.T.);
#7000=EDGE_CURVE('',#5678,#5606,#3202,.T.);
#7001=EDGE_CURVE('',#5679,#5605,#3203,.T.);
#7002=EDGE_CURVE('',#5680,#5604,#3204,.T.);
#7003=EDGE_CURVE('',#5686,#5665,#3205,.T.);
#7004=EDGE_CURVE('',#5681,#5686,#3206,.T.);
#7005=EDGE_CURVE('',#5687,#5686,#3207,.T.);
#7006=EDGE_CURVE('',#5682,#5687,#3208,.T.);
#7007=EDGE_CURVE('',#5688,#5687,#3209,.T.);
#7008=EDGE_CURVE('',#5683,#5688,#3210,.T.);
#7009=EDGE_CURVE('',#5689,#5688,#3211,.T.);
#7010=EDGE_CURVE('',#5684,#5689,#3212,.T.);
#7011=EDGE_CURVE('',#5690,#5689,#3213,.T.);
#7012=EDGE_CURVE('',#5685,#5690,#3214,.T.);
#7013=EDGE_CURVE('',#5691,#5690,#3215,.T.);
#7014=EDGE_CURVE('',#5675,#5691,#3216,.T.);
#7015=EDGE_CURVE('',#5674,#5691,#3217,.T.);
#7016=EDGE_CURVE('',#5657,#5692,#3218,.T.);
#7017=EDGE_CURVE('',#5693,#5692,#3219,.T.);
#7018=EDGE_CURVE('',#5694,#5693,#3220,.T.);
#7019=EDGE_CURVE('',#5695,#5694,#3221,.T.);
#7020=EDGE_CURVE('',#5695,#5566,#3222,.T.);
#7021=EDGE_CURVE('',#5656,#5696,#3223,.T.);
#7022=EDGE_CURVE('',#5692,#5696,#3224,.T.);
#7023=EDGE_CURVE('',#5697,#5695,#3225,.T.);
#7024=EDGE_CURVE('',#5697,#5567,#3226,.T.);
#7025=EDGE_CURVE('',#5655,#5698,#3227,.T.);
#7026=EDGE_CURVE('',#5696,#5698,#3228,.T.);
#7027=EDGE_CURVE('',#5654,#5699,#3229,.T.);
#7028=EDGE_CURVE('',#5698,#5699,#3230,.T.);
#7029=EDGE_CURVE('',#5653,#5700,#3231,.T.);
#7030=EDGE_CURVE('',#5699,#5700,#3232,.T.);
#7031=EDGE_CURVE('',#5652,#5701,#3233,.T.);
#7032=EDGE_CURVE('',#5700,#5701,#3234,.T.);
#7033=EDGE_CURVE('',#5702,#5651,#3235,.T.);
#7034=EDGE_CURVE('',#5701,#5702,#3236,.T.);
#7035=EDGE_CURVE('',#5703,#5704,#3237,.T.);
#7036=EDGE_CURVE('',#5704,#5705,#3238,.T.);
#7037=EDGE_CURVE('',#5705,#5706,#3239,.T.);
#7038=EDGE_CURVE('',#5706,#5707,#3240,.T.);
#7039=EDGE_CURVE('',#5707,#5708,#3241,.T.);
#7040=EDGE_CURVE('',#5708,#5697,#3242,.T.);
#7041=EDGE_CURVE('',#5694,#5709,#3243,.T.);
#7042=EDGE_CURVE('',#5709,#5710,#3244,.T.);
#7043=EDGE_CURVE('',#5710,#5711,#3245,.T.);
#7044=EDGE_CURVE('',#5711,#5712,#3246,.T.);
#7045=EDGE_CURVE('',#5712,#5713,#3247,.T.);
#7046=EDGE_CURVE('',#5713,#5703,#3248,.T.);
#7047=EDGE_CURVE('',#5705,#5571,#3249,.T.);
#7048=EDGE_CURVE('',#5572,#5704,#3250,.T.);
#7049=EDGE_CURVE('',#5706,#5570,#3251,.T.);
#7050=EDGE_CURVE('',#5707,#5569,#3252,.T.);
#7051=EDGE_CURVE('',#5708,#5568,#3253,.T.);
#7052=EDGE_CURVE('',#5714,#5693,#3254,.T.);
#7053=EDGE_CURVE('',#5709,#5714,#3255,.T.);
#7054=EDGE_CURVE('',#5715,#5714,#3256,.T.);
#7055=EDGE_CURVE('',#5710,#5715,#3257,.T.);
#7056=EDGE_CURVE('',#5716,#5715,#3258,.T.);
#7057=EDGE_CURVE('',#5711,#5716,#3259,.T.);
#7058=EDGE_CURVE('',#5717,#5716,#3260,.T.);
#7059=EDGE_CURVE('',#5712,#5717,#3261,.T.);
#7060=EDGE_CURVE('',#5718,#5717,#3262,.T.);
#7061=EDGE_CURVE('',#5713,#5718,#3263,.T.);
#7062=EDGE_CURVE('',#5719,#5718,#3264,.T.);
#7063=EDGE_CURVE('',#5703,#5719,#3265,.T.);
#7064=EDGE_CURVE('',#5702,#5719,#3266,.T.);
#7065=EDGE_CURVE('',#5643,#5720,#3267,.T.);
#7066=EDGE_CURVE('',#5721,#5720,#3268,.T.);
#7067=EDGE_CURVE('',#5722,#5721,#3269,.T.);
#7068=EDGE_CURVE('',#5723,#5722,#3270,.T.);
#7069=EDGE_CURVE('',#5723,#5584,#3271,.T.);
#7070=EDGE_CURVE('',#5642,#5724,#3272,.T.);
#7071=EDGE_CURVE('',#5720,#5724,#3273,.T.);
#7072=EDGE_CURVE('',#5725,#5723,#3274,.T.);
#7073=EDGE_CURVE('',#5725,#5585,#3275,.T.);
#7074=EDGE_CURVE('',#5641,#5726,#3276,.T.);
#7075=EDGE_CURVE('',#5724,#5726,#3277,.T.);
#7076=EDGE_CURVE('',#5640,#5727,#3278,.T.);
#7077=EDGE_CURVE('',#5726,#5727,#3279,.T.);
#7078=EDGE_CURVE('',#5639,#5728,#3280,.T.);
#7079=EDGE_CURVE('',#5727,#5728,#3281,.T.);
#7080=EDGE_CURVE('',#5638,#5729,#3282,.T.);
#7081=EDGE_CURVE('',#5728,#5729,#3283,.T.);
#7082=EDGE_CURVE('',#5730,#5637,#3284,.T.);
#7083=EDGE_CURVE('',#5729,#5730,#3285,.T.);
#7084=EDGE_CURVE('',#5731,#5732,#3286,.T.);
#7085=EDGE_CURVE('',#5732,#5733,#3287,.T.);
#7086=EDGE_CURVE('',#5733,#5734,#3288,.T.);
#7087=EDGE_CURVE('',#5734,#5735,#3289,.T.);
#7088=EDGE_CURVE('',#5735,#5736,#3290,.T.);
#7089=EDGE_CURVE('',#5736,#5725,#3291,.T.);
#7090=EDGE_CURVE('',#5722,#5737,#3292,.T.);
#7091=EDGE_CURVE('',#5737,#5738,#3293,.T.);
#7092=EDGE_CURVE('',#5738,#5739,#3294,.T.);
#7093=EDGE_CURVE('',#5739,#5740,#3295,.T.);
#7094=EDGE_CURVE('',#5740,#5741,#3296,.T.);
#7095=EDGE_CURVE('',#5741,#5731,#3297,.T.);
#7096=EDGE_CURVE('',#5733,#5589,#3298,.T.);
#7097=EDGE_CURVE('',#5590,#5732,#3299,.T.);
#7098=EDGE_CURVE('',#5734,#5588,#3300,.T.);
#7099=EDGE_CURVE('',#5735,#5587,#3301,.T.);
#7100=EDGE_CURVE('',#5736,#5586,#3302,.T.);
#7101=EDGE_CURVE('',#5742,#5721,#3303,.T.);
#7102=EDGE_CURVE('',#5737,#5742,#3304,.T.);
#7103=EDGE_CURVE('',#5743,#5742,#3305,.T.);
#7104=EDGE_CURVE('',#5738,#5743,#3306,.T.);
#7105=EDGE_CURVE('',#5744,#5743,#3307,.T.);
#7106=EDGE_CURVE('',#5739,#5744,#3308,.T.);
#7107=EDGE_CURVE('',#5745,#5744,#3309,.T.);
#7108=EDGE_CURVE('',#5740,#5745,#3310,.T.);
#7109=EDGE_CURVE('',#5746,#5745,#3311,.T.);
#7110=EDGE_CURVE('',#5741,#5746,#3312,.T.);
#7111=EDGE_CURVE('',#5747,#5746,#3313,.T.);
#7112=EDGE_CURVE('',#5731,#5747,#3314,.T.);
#7113=EDGE_CURVE('',#5730,#5747,#3315,.T.);
#7114=EDGE_CURVE('',#5636,#5748,#3316,.T.);
#7115=EDGE_CURVE('',#5749,#5748,#3317,.T.);
#7116=EDGE_CURVE('',#5750,#5749,#3318,.T.);
#7117=EDGE_CURVE('',#5751,#5750,#3319,.T.);
#7118=EDGE_CURVE('',#5751,#5593,#3320,.T.);
#7119=EDGE_CURVE('',#5635,#5752,#3321,.T.);
#7120=EDGE_CURVE('',#5748,#5752,#3322,.T.);
#7121=EDGE_CURVE('',#5753,#5751,#3323,.T.);
#7122=EDGE_CURVE('',#5753,#5594,#3324,.T.);
#7123=EDGE_CURVE('',#5634,#5754,#3325,.T.);
#7124=EDGE_CURVE('',#5752,#5754,#3326,.T.);
#7125=EDGE_CURVE('',#5633,#5755,#3327,.T.);
#7126=EDGE_CURVE('',#5754,#5755,#3328,.T.);
#7127=EDGE_CURVE('',#5632,#5756,#3329,.T.);
#7128=EDGE_CURVE('',#5755,#5756,#3330,.T.);
#7129=EDGE_CURVE('',#5631,#5757,#3331,.T.);
#7130=EDGE_CURVE('',#5756,#5757,#3332,.T.);
#7131=EDGE_CURVE('',#5758,#5630,#3333,.T.);
#7132=EDGE_CURVE('',#5757,#5758,#3334,.T.);
#7133=EDGE_CURVE('',#5759,#5760,#3335,.T.);
#7134=EDGE_CURVE('',#5760,#5761,#3336,.T.);
#7135=EDGE_CURVE('',#5761,#5762,#3337,.T.);
#7136=EDGE_CURVE('',#5762,#5763,#3338,.T.);
#7137=EDGE_CURVE('',#5763,#5764,#3339,.T.);
#7138=EDGE_CURVE('',#5764,#5753,#3340,.T.);
#7139=EDGE_CURVE('',#5750,#5765,#3341,.T.);
#7140=EDGE_CURVE('',#5765,#5766,#3342,.T.);
#7141=EDGE_CURVE('',#5766,#5767,#3343,.T.);
#7142=EDGE_CURVE('',#5767,#5768,#3344,.T.);
#7143=EDGE_CURVE('',#5768,#5769,#3345,.T.);
#7144=EDGE_CURVE('',#5769,#5759,#3346,.T.);
#7145=EDGE_CURVE('',#5761,#5598,#3347,.T.);
#7146=EDGE_CURVE('',#5599,#5760,#3348,.T.);
#7147=EDGE_CURVE('',#5762,#5597,#3349,.T.);
#7148=EDGE_CURVE('',#5763,#5596,#3350,.T.);
#7149=EDGE_CURVE('',#5764,#5595,#3351,.T.);
#7150=EDGE_CURVE('',#5770,#5749,#3352,.T.);
#7151=EDGE_CURVE('',#5765,#5770,#3353,.T.);
#7152=EDGE_CURVE('',#5771,#5770,#3354,.T.);
#7153=EDGE_CURVE('',#5766,#5771,#3355,.T.);
#7154=EDGE_CURVE('',#5772,#5771,#3356,.T.);
#7155=EDGE_CURVE('',#5767,#5772,#3357,.T.);
#7156=EDGE_CURVE('',#5773,#5772,#3358,.T.);
#7157=EDGE_CURVE('',#5768,#5773,#3359,.T.);
#7158=EDGE_CURVE('',#5774,#5773,#3360,.T.);
#7159=EDGE_CURVE('',#5769,#5774,#3361,.T.);
#7160=EDGE_CURVE('',#5775,#5774,#3362,.T.);
#7161=EDGE_CURVE('',#5759,#5775,#3363,.T.);
#7162=EDGE_CURVE('',#5758,#5775,#3364,.T.);
#7163=EDGE_CURVE('',#5650,#5776,#3365,.T.);
#7164=EDGE_CURVE('',#5777,#5776,#3366,.T.);
#7165=EDGE_CURVE('',#5778,#5777,#3367,.T.);
#7166=EDGE_CURVE('',#5779,#5778,#3368,.T.);
#7167=EDGE_CURVE('',#5779,#5575,#3369,.T.);
#7168=EDGE_CURVE('',#5649,#5780,#3370,.T.);
#7169=EDGE_CURVE('',#5776,#5780,#3371,.T.);
#7170=EDGE_CURVE('',#5781,#5779,#3372,.T.);
#7171=EDGE_CURVE('',#5781,#5576,#3373,.T.);
#7172=EDGE_CURVE('',#5648,#5782,#3374,.T.);
#7173=EDGE_CURVE('',#5780,#5782,#3375,.T.);
#7174=EDGE_CURVE('',#5647,#5783,#3376,.T.);
#7175=EDGE_CURVE('',#5782,#5783,#3377,.T.);
#7176=EDGE_CURVE('',#5646,#5784,#3378,.T.);
#7177=EDGE_CURVE('',#5783,#5784,#3379,.T.);
#7178=EDGE_CURVE('',#5645,#5785,#3380,.T.);
#7179=EDGE_CURVE('',#5784,#5785,#3381,.T.);
#7180=EDGE_CURVE('',#5786,#5644,#3382,.T.);
#7181=EDGE_CURVE('',#5785,#5786,#3383,.T.);
#7182=EDGE_CURVE('',#5787,#5788,#3384,.T.);
#7183=EDGE_CURVE('',#5788,#5789,#3385,.T.);
#7184=EDGE_CURVE('',#5789,#5790,#3386,.T.);
#7185=EDGE_CURVE('',#5790,#5791,#3387,.T.);
#7186=EDGE_CURVE('',#5791,#5792,#3388,.T.);
#7187=EDGE_CURVE('',#5792,#5781,#3389,.T.);
#7188=EDGE_CURVE('',#5778,#5793,#3390,.T.);
#7189=EDGE_CURVE('',#5793,#5794,#3391,.T.);
#7190=EDGE_CURVE('',#5794,#5795,#3392,.T.);
#7191=EDGE_CURVE('',#5795,#5796,#3393,.T.);
#7192=EDGE_CURVE('',#5796,#5797,#3394,.T.);
#7193=EDGE_CURVE('',#5797,#5787,#3395,.T.);
#7194=EDGE_CURVE('',#5789,#5580,#3396,.T.);
#7195=EDGE_CURVE('',#5581,#5788,#3397,.T.);
#7196=EDGE_CURVE('',#5790,#5579,#3398,.T.);
#7197=EDGE_CURVE('',#5791,#5578,#3399,.T.);
#7198=EDGE_CURVE('',#5792,#5577,#3400,.T.);
#7199=EDGE_CURVE('',#5798,#5777,#3401,.T.);
#7200=EDGE_CURVE('',#5793,#5798,#3402,.T.);
#7201=EDGE_CURVE('',#5799,#5798,#3403,.T.);
#7202=EDGE_CURVE('',#5794,#5799,#3404,.T.);
#7203=EDGE_CURVE('',#5800,#5799,#3405,.T.);
#7204=EDGE_CURVE('',#5795,#5800,#3406,.T.);
#7205=EDGE_CURVE('',#5801,#5800,#3407,.T.);
#7206=EDGE_CURVE('',#5796,#5801,#3408,.T.);
#7207=EDGE_CURVE('',#5802,#5801,#3409,.T.);
#7208=EDGE_CURVE('',#5797,#5802,#3410,.T.);
#7209=EDGE_CURVE('',#5803,#5802,#3411,.T.);
#7210=EDGE_CURVE('',#5787,#5803,#3412,.T.);
#7211=EDGE_CURVE('',#5786,#5803,#3413,.T.);
#7212=EDGE_CURVE('',#5622,#5804,#3414,.T.);
#7213=EDGE_CURVE('',#5805,#5804,#3415,.T.);
#7214=EDGE_CURVE('',#5806,#5805,#3416,.T.);
#7215=EDGE_CURVE('',#5807,#5806,#3417,.T.);
#7216=EDGE_CURVE('',#5807,#5556,#3418,.T.);
#7217=EDGE_CURVE('',#5663,#5808,#3419,.T.);
#7218=EDGE_CURVE('',#5804,#5808,#3420,.T.);
#7219=EDGE_CURVE('',#5809,#5807,#3421,.T.);
#7220=EDGE_CURVE('',#5809,#5558,#3422,.T.);
#7221=EDGE_CURVE('',#5662,#5810,#3423,.T.);
#7222=EDGE_CURVE('',#5808,#5810,#3424,.T.);
#7223=EDGE_CURVE('',#5661,#5811,#3425,.T.);
#7224=EDGE_CURVE('',#5810,#5811,#3426,.T.);
#7225=EDGE_CURVE('',#5660,#5812,#3427,.T.);
#7226=EDGE_CURVE('',#5811,#5812,#3428,.T.);
#7227=EDGE_CURVE('',#5659,#5813,#3429,.T.);
#7228=EDGE_CURVE('',#5812,#5813,#3430,.T.);
#7229=EDGE_CURVE('',#5814,#5658,#3431,.T.);
#7230=EDGE_CURVE('',#5813,#5814,#3432,.T.);
#7231=EDGE_CURVE('',#5815,#5816,#3433,.T.);
#7232=EDGE_CURVE('',#5816,#5817,#3434,.T.);
#7233=EDGE_CURVE('',#5817,#5818,#3435,.T.);
#7234=EDGE_CURVE('',#5818,#5819,#3436,.T.);
#7235=EDGE_CURVE('',#5819,#5820,#3437,.T.);
#7236=EDGE_CURVE('',#5820,#5809,#3438,.T.);
#7237=EDGE_CURVE('',#5806,#5821,#3439,.T.);
#7238=EDGE_CURVE('',#5821,#5822,#3440,.T.);
#7239=EDGE_CURVE('',#5822,#5823,#3441,.T.);
#7240=EDGE_CURVE('',#5823,#5824,#3442,.T.);
#7241=EDGE_CURVE('',#5824,#5825,#3443,.T.);
#7242=EDGE_CURVE('',#5825,#5815,#3444,.T.);
#7243=EDGE_CURVE('',#5817,#5562,#3445,.T.);
#7244=EDGE_CURVE('',#5563,#5816,#3446,.T.);
#7245=EDGE_CURVE('',#5818,#5561,#3447,.T.);
#7246=EDGE_CURVE('',#5819,#5560,#3448,.T.);
#7247=EDGE_CURVE('',#5820,#5559,#3449,.T.);
#7248=EDGE_CURVE('',#5826,#5805,#3450,.T.);
#7249=EDGE_CURVE('',#5821,#5826,#3451,.T.);
#7250=EDGE_CURVE('',#5827,#5826,#3452,.T.);
#7251=EDGE_CURVE('',#5822,#5827,#3453,.T.);
#7252=EDGE_CURVE('',#5828,#5827,#3454,.T.);
#7253=EDGE_CURVE('',#5823,#5828,#3455,.T.);
#7254=EDGE_CURVE('',#5829,#5828,#3456,.T.);
#7255=EDGE_CURVE('',#5824,#5829,#3457,.T.);
#7256=EDGE_CURVE('',#5830,#5829,#3458,.T.);
#7257=EDGE_CURVE('',#5825,#5830,#3459,.T.);
#7258=EDGE_CURVE('',#5831,#5830,#3460,.T.);
#7259=EDGE_CURVE('',#5815,#5831,#3461,.T.);
#7260=EDGE_CURVE('',#5814,#5831,#3462,.T.);
#7261=EDGE_CURVE('',#5832,#5833,#3463,.T.);
#7262=EDGE_CURVE('',#5833,#5834,#3464,.T.);
#7263=EDGE_CURVE('',#5834,#5835,#3465,.T.);
#7264=EDGE_CURVE('',#5835,#5832,#3466,.T.);
#7265=EDGE_CURVE('',#5836,#5837,#3467,.T.);
#7266=EDGE_CURVE('',#5837,#5833,#4923,.T.);
#7267=EDGE_CURVE('',#5832,#5836,#4924,.T.);
#7268=EDGE_CURVE('',#5838,#5839,#3468,.T.);
#7269=EDGE_CURVE('',#5839,#5837,#3469,.T.);
#7270=EDGE_CURVE('',#5836,#5838,#3470,.T.);
#7271=EDGE_CURVE('',#5834,#5839,#4925,.T.);
#7272=EDGE_CURVE('',#5838,#5835,#4926,.T.);
#7273=EDGE_CURVE('',#5840,#5832,#3471,.T.);
#7274=EDGE_CURVE('',#5841,#5840,#4927,.T.);
#7275=EDGE_CURVE('',#5841,#5836,#3472,.T.);
#7276=EDGE_CURVE('',#5842,#5835,#3473,.T.);
#7277=EDGE_CURVE('',#5840,#5842,#3474,.T.);
#7278=EDGE_CURVE('',#5843,#5840,#3475,.T.);
#7279=EDGE_CURVE('',#5842,#5844,#3476,.T.);
#7280=EDGE_CURVE('',#5844,#5843,#3477,.T.);
#7281=EDGE_CURVE('',#5845,#5841,#3478,.T.);
#7282=EDGE_CURVE('',#5843,#5845,#4928,.T.);
#7283=EDGE_CURVE('',#5846,#5847,#3479,.T.);
#7284=EDGE_CURVE('',#5847,#5841,#3480,.T.);
#7285=EDGE_CURVE('',#5845,#5846,#3481,.T.);
#7286=EDGE_CURVE('',#5842,#5847,#4929,.T.);
#7287=EDGE_CURVE('',#5846,#5844,#4930,.T.);
#7288=EDGE_CURVE('',#5847,#5838,#3482,.T.);
#7289=EDGE_CURVE('',#5848,#5849,#3483,.T.);
#7290=EDGE_CURVE('',#5848,#5850,#3484,.T.);
#7291=EDGE_CURVE('',#5850,#5851,#3485,.T.);
#7292=EDGE_CURVE('',#5849,#5851,#3486,.T.);
#7293=EDGE_CURVE('',#5852,#5848,#3487,.T.);
#7294=EDGE_CURVE('',#5852,#5853,#3488,.T.);
#7295=EDGE_CURVE('',#5853,#5850,#3489,.T.);
#7296=EDGE_CURVE('',#5854,#5852,#3490,.T.);
#7297=EDGE_CURVE('',#5854,#5855,#3491,.T.);
#7298=EDGE_CURVE('',#5855,#5853,#3492,.T.);
#7299=EDGE_CURVE('',#5856,#5854,#3493,.T.);
#7300=EDGE_CURVE('',#5856,#5857,#3494,.T.);
#7301=EDGE_CURVE('',#5857,#5855,#3495,.T.);
#7302=EDGE_CURVE('',#5858,#5856,#3496,.T.);
#7303=EDGE_CURVE('',#5858,#5859,#3497,.T.);
#7304=EDGE_CURVE('',#5859,#5857,#3498,.T.);
#7305=EDGE_CURVE('',#5849,#5858,#3499,.T.);
#7306=EDGE_CURVE('',#5851,#5859,#3500,.T.);
#7307=EDGE_CURVE('',#5860,#5860,#4931,.T.);
#7308=EDGE_CURVE('',#5861,#5861,#4932,.T.);
#7309=EDGE_CURVE('',#5861,#5860,#3501,.T.);
#7310=EDGE_CURVE('',#5862,#5862,#4933,.F.);
#7311=EDGE_CURVE('',#5862,#5861,#3502,.T.);
#7312=EDGE_CURVE('',#5863,#5863,#4934,.T.);
#7313=EDGE_CURVE('',#5863,#5862,#3503,.T.);
#7314=EDGE_CURVE('',#5864,#5864,#4935,.T.);
#7315=EDGE_CURVE('',#5865,#5865,#4936,.T.);
#7316=EDGE_CURVE('',#5865,#5864,#3504,.T.);
#7317=EDGE_CURVE('',#5866,#5866,#4937,.T.);
#7318=EDGE_CURVE('',#5866,#5865,#3505,.T.);
#7319=EDGE_CURVE('',#5867,#5867,#4938,.T.);
#7320=EDGE_CURVE('',#5867,#5866,#3506,.T.);
#7321=EDGE_CURVE('',#5868,#5868,#4939,.T.);
#7322=EDGE_CURVE('',#5869,#5869,#4940,.F.);
#7323=EDGE_CURVE('',#5869,#5868,#3507,.T.);
#7324=EDGE_CURVE('',#5870,#5870,#4941,.F.);
#7325=EDGE_CURVE('',#5870,#5869,#3508,.T.);
#7326=EDGE_CURVE('',#5871,#5871,#4942,.T.);
#7327=EDGE_CURVE('',#5871,#5870,#3509,.T.);
#7328=EDGE_CURVE('',#5872,#5873,#3510,.T.);
#7329=EDGE_CURVE('',#5873,#5874,#3511,.T.);
#7330=EDGE_CURVE('',#5874,#5875,#3512,.T.);
#7331=EDGE_CURVE('',#5872,#5875,#3513,.T.);
#7332=EDGE_CURVE('',#5873,#5876,#3514,.T.);
#7333=EDGE_CURVE('',#5876,#5877,#3515,.T.);
#7334=EDGE_CURVE('',#5877,#5874,#3516,.T.);
#7335=EDGE_CURVE('',#5876,#5878,#3517,.T.);
#7336=EDGE_CURVE('',#5878,#5879,#3518,.T.);
#7337=EDGE_CURVE('',#5879,#5877,#3519,.T.);
#7338=EDGE_CURVE('',#5878,#5880,#3520,.T.);
#7339=EDGE_CURVE('',#5880,#5881,#3521,.T.);
#7340=EDGE_CURVE('',#5881,#5879,#3522,.T.);
#7341=EDGE_CURVE('',#5880,#5882,#3523,.T.);
#7342=EDGE_CURVE('',#5882,#5883,#3524,.T.);
#7343=EDGE_CURVE('',#5883,#5881,#3525,.T.);
#7344=EDGE_CURVE('',#5882,#5872,#3526,.T.);
#7345=EDGE_CURVE('',#5875,#5883,#3527,.T.);
#7346=ORIENTED_EDGE('',*,*,#5884,.F.);
#7347=ORIENTED_EDGE('',*,*,#5885,.T.);
#7348=ORIENTED_EDGE('',*,*,#5886,.F.);
#7349=ORIENTED_EDGE('',*,*,#5885,.F.);
#7350=ORIENTED_EDGE('',*,*,#5887,.F.);
#7351=ORIENTED_EDGE('',*,*,#5888,.T.);
#7352=ORIENTED_EDGE('',*,*,#5889,.F.);
#7353=ORIENTED_EDGE('',*,*,#5888,.F.);
#7354=ORIENTED_EDGE('',*,*,#5890,.F.);
#7355=ORIENTED_EDGE('',*,*,#5891,.T.);
#7356=ORIENTED_EDGE('',*,*,#5892,.F.);
#7357=ORIENTED_EDGE('',*,*,#5891,.F.);
#7358=ORIENTED_EDGE('',*,*,#5893,.F.);
#7359=ORIENTED_EDGE('',*,*,#5894,.T.);
#7360=ORIENTED_EDGE('',*,*,#5895,.F.);
#7361=ORIENTED_EDGE('',*,*,#5894,.F.);
#7362=ORIENTED_EDGE('',*,*,#5896,.F.);
#7363=ORIENTED_EDGE('',*,*,#5897,.T.);
#7364=ORIENTED_EDGE('',*,*,#5898,.F.);
#7365=ORIENTED_EDGE('',*,*,#5897,.F.);
#7366=ORIENTED_EDGE('',*,*,#5899,.F.);
#7367=ORIENTED_EDGE('',*,*,#5900,.T.);
#7368=ORIENTED_EDGE('',*,*,#5901,.F.);
#7369=ORIENTED_EDGE('',*,*,#5900,.F.);
#7370=ORIENTED_EDGE('',*,*,#5902,.T.);
#7371=ORIENTED_EDGE('',*,*,#5903,.T.);
#7372=ORIENTED_EDGE('',*,*,#5904,.F.);
#7373=ORIENTED_EDGE('',*,*,#5905,.F.);
#7374=ORIENTED_EDGE('',*,*,#5906,.T.);
#7375=ORIENTED_EDGE('',*,*,#5905,.T.);
#7376=ORIENTED_EDGE('',*,*,#5907,.F.);
#7377=ORIENTED_EDGE('',*,*,#5908,.F.);
#7378=ORIENTED_EDGE('',*,*,#5909,.T.);
#7379=ORIENTED_EDGE('',*,*,#5908,.T.);
#7380=ORIENTED_EDGE('',*,*,#5910,.F.);
#7381=ORIENTED_EDGE('',*,*,#5911,.F.);
#7382=ORIENTED_EDGE('',*,*,#5912,.T.);
#7383=ORIENTED_EDGE('',*,*,#5911,.T.);
#7384=ORIENTED_EDGE('',*,*,#5913,.F.);
#7385=ORIENTED_EDGE('',*,*,#5903,.F.);
#7386=ORIENTED_EDGE('',*,*,#5913,.T.);
#7387=ORIENTED_EDGE('',*,*,#5910,.T.);
#7388=ORIENTED_EDGE('',*,*,#5907,.T.);
#7389=ORIENTED_EDGE('',*,*,#5904,.T.);
#7390=ORIENTED_EDGE('',*,*,#5886,.T.);
#7391=ORIENTED_EDGE('',*,*,#5889,.T.);
#7392=ORIENTED_EDGE('',*,*,#5892,.T.);
#7393=ORIENTED_EDGE('',*,*,#5895,.T.);
#7394=ORIENTED_EDGE('',*,*,#5898,.T.);
#7395=ORIENTED_EDGE('',*,*,#5901,.T.);
#7396=ORIENTED_EDGE('',*,*,#5912,.F.);
#7397=ORIENTED_EDGE('',*,*,#5902,.F.);
#7398=ORIENTED_EDGE('',*,*,#5906,.F.);
#7399=ORIENTED_EDGE('',*,*,#5909,.F.);
#7400=ORIENTED_EDGE('',*,*,#5884,.T.);
#7401=ORIENTED_EDGE('',*,*,#5887,.T.);
#7402=ORIENTED_EDGE('',*,*,#5890,.T.);
#7403=ORIENTED_EDGE('',*,*,#5893,.T.);
#7404=ORIENTED_EDGE('',*,*,#5896,.T.);
#7405=ORIENTED_EDGE('',*,*,#5899,.T.);
#7406=ORIENTED_EDGE('',*,*,#5914,.T.);
#7407=ORIENTED_EDGE('',*,*,#5915,.T.);
#7408=ORIENTED_EDGE('',*,*,#5916,.F.);
#7409=ORIENTED_EDGE('',*,*,#5917,.F.);
#7410=ORIENTED_EDGE('',*,*,#5918,.T.);
#7411=ORIENTED_EDGE('',*,*,#5917,.T.);
#7412=ORIENTED_EDGE('',*,*,#5919,.F.);
#7413=ORIENTED_EDGE('',*,*,#5920,.F.);
#7414=ORIENTED_EDGE('',*,*,#5921,.T.);
#7415=ORIENTED_EDGE('',*,*,#5920,.T.);
#7416=ORIENTED_EDGE('',*,*,#5922,.F.);
#7417=ORIENTED_EDGE('',*,*,#5923,.F.);
#7418=ORIENTED_EDGE('',*,*,#5924,.T.);
#7419=ORIENTED_EDGE('',*,*,#5923,.T.);
#7420=ORIENTED_EDGE('',*,*,#5925,.F.);
#7421=ORIENTED_EDGE('',*,*,#5915,.F.);
#7422=ORIENTED_EDGE('',*,*,#5925,.T.);
#7423=ORIENTED_EDGE('',*,*,#5922,.T.);
#7424=ORIENTED_EDGE('',*,*,#5919,.T.);
#7425=ORIENTED_EDGE('',*,*,#5916,.T.);
#7426=ORIENTED_EDGE('',*,*,#5924,.F.);
#7427=ORIENTED_EDGE('',*,*,#5914,.F.);
#7428=ORIENTED_EDGE('',*,*,#5918,.F.);
#7429=ORIENTED_EDGE('',*,*,#5921,.F.);
#7430=ORIENTED_EDGE('',*,*,#5926,.T.);
#7431=ORIENTED_EDGE('',*,*,#5927,.T.);
#7432=ORIENTED_EDGE('',*,*,#5928,.F.);
#7433=ORIENTED_EDGE('',*,*,#5929,.F.);
#7434=ORIENTED_EDGE('',*,*,#5930,.T.);
#7435=ORIENTED_EDGE('',*,*,#5929,.T.);
#7436=ORIENTED_EDGE('',*,*,#5931,.F.);
#7437=ORIENTED_EDGE('',*,*,#5932,.F.);
#7438=ORIENTED_EDGE('',*,*,#5933,.T.);
#7439=ORIENTED_EDGE('',*,*,#5932,.T.);
#7440=ORIENTED_EDGE('',*,*,#5934,.F.);
#7441=ORIENTED_EDGE('',*,*,#5935,.F.);
#7442=ORIENTED_EDGE('',*,*,#5936,.T.);
#7443=ORIENTED_EDGE('',*,*,#5935,.T.);
#7444=ORIENTED_EDGE('',*,*,#5937,.F.);
#7445=ORIENTED_EDGE('',*,*,#5927,.F.);
#7446=ORIENTED_EDGE('',*,*,#5937,.T.);
#7447=ORIENTED_EDGE('',*,*,#5934,.T.);
#7448=ORIENTED_EDGE('',*,*,#5931,.T.);
#7449=ORIENTED_EDGE('',*,*,#5928,.T.);
#7450=ORIENTED_EDGE('',*,*,#5936,.F.);
#7451=ORIENTED_EDGE('',*,*,#5926,.F.);
#7452=ORIENTED_EDGE('',*,*,#5930,.F.);
#7453=ORIENTED_EDGE('',*,*,#5933,.F.);
#7454=ORIENTED_EDGE('',*,*,#5938,.F.);
#7455=ORIENTED_EDGE('',*,*,#5939,.T.);
#7456=ORIENTED_EDGE('',*,*,#5940,.T.);
#7457=ORIENTED_EDGE('',*,*,#5939,.F.);
#7458=ORIENTED_EDGE('',*,*,#5941,.F.);
#7459=ORIENTED_EDGE('',*,*,#5942,.T.);
#7460=ORIENTED_EDGE('',*,*,#5943,.T.);
#7461=ORIENTED_EDGE('',*,*,#5942,.F.);
#7462=ORIENTED_EDGE('',*,*,#5941,.T.);
#7463=ORIENTED_EDGE('',*,*,#5938,.T.);
#7464=ORIENTED_EDGE('',*,*,#5943,.F.);
#7465=ORIENTED_EDGE('',*,*,#5940,.F.);
#7466=ORIENTED_EDGE('',*,*,#5944,.F.);
#7467=ORIENTED_EDGE('',*,*,#5945,.T.);
#7468=ORIENTED_EDGE('',*,*,#5946,.T.);
#7469=ORIENTED_EDGE('',*,*,#5945,.F.);
#7470=ORIENTED_EDGE('',*,*,#5947,.F.);
#7471=ORIENTED_EDGE('',*,*,#5948,.T.);
#7472=ORIENTED_EDGE('',*,*,#5949,.T.);
#7473=ORIENTED_EDGE('',*,*,#5948,.F.);
#7474=ORIENTED_EDGE('',*,*,#5947,.T.);
#7475=ORIENTED_EDGE('',*,*,#5944,.T.);
#7476=ORIENTED_EDGE('',*,*,#5949,.F.);
#7477=ORIENTED_EDGE('',*,*,#5946,.F.);
#7478=ORIENTED_EDGE('',*,*,#5950,.F.);
#7479=ORIENTED_EDGE('',*,*,#5951,.T.);
#7480=ORIENTED_EDGE('',*,*,#5952,.T.);
#7481=ORIENTED_EDGE('',*,*,#5951,.F.);
#7482=ORIENTED_EDGE('',*,*,#5953,.F.);
#7483=ORIENTED_EDGE('',*,*,#5954,.T.);
#7484=ORIENTED_EDGE('',*,*,#5955,.T.);
#7485=ORIENTED_EDGE('',*,*,#5954,.F.);
#7486=ORIENTED_EDGE('',*,*,#5953,.T.);
#7487=ORIENTED_EDGE('',*,*,#5950,.T.);
#7488=ORIENTED_EDGE('',*,*,#5955,.F.);
#7489=ORIENTED_EDGE('',*,*,#5952,.F.);
#7490=ORIENTED_EDGE('',*,*,#5956,.F.);
#7491=ORIENTED_EDGE('',*,*,#5957,.T.);
#7492=ORIENTED_EDGE('',*,*,#5958,.T.);
#7493=ORIENTED_EDGE('',*,*,#5957,.F.);
#7494=ORIENTED_EDGE('',*,*,#5959,.F.);
#7495=ORIENTED_EDGE('',*,*,#5960,.T.);
#7496=ORIENTED_EDGE('',*,*,#5961,.T.);
#7497=ORIENTED_EDGE('',*,*,#5960,.F.);
#7498=ORIENTED_EDGE('',*,*,#5959,.T.);
#7499=ORIENTED_EDGE('',*,*,#5956,.T.);
#7500=ORIENTED_EDGE('',*,*,#5961,.F.);
#7501=ORIENTED_EDGE('',*,*,#5958,.F.);
#7502=ORIENTED_EDGE('',*,*,#5962,.F.);
#7503=ORIENTED_EDGE('',*,*,#5963,.T.);
#7504=ORIENTED_EDGE('',*,*,#5964,.F.);
#7505=ORIENTED_EDGE('',*,*,#5963,.F.);
#7506=ORIENTED_EDGE('',*,*,#5965,.F.);
#7507=ORIENTED_EDGE('',*,*,#5966,.T.);
#7508=ORIENTED_EDGE('',*,*,#5967,.F.);
#7509=ORIENTED_EDGE('',*,*,#5966,.F.);
#7510=ORIENTED_EDGE('',*,*,#5968,.F.);
#7511=ORIENTED_EDGE('',*,*,#5969,.T.);
#7512=ORIENTED_EDGE('',*,*,#5970,.F.);
#7513=ORIENTED_EDGE('',*,*,#5969,.F.);
#7514=ORIENTED_EDGE('',*,*,#5971,.F.);
#7515=ORIENTED_EDGE('',*,*,#5972,.T.);
#7516=ORIENTED_EDGE('',*,*,#5973,.F.);
#7517=ORIENTED_EDGE('',*,*,#5972,.F.);
#7518=ORIENTED_EDGE('',*,*,#5974,.F.);
#7519=ORIENTED_EDGE('',*,*,#5975,.T.);
#7520=ORIENTED_EDGE('',*,*,#5976,.F.);
#7521=ORIENTED_EDGE('',*,*,#5975,.F.);
#7522=ORIENTED_EDGE('',*,*,#5977,.F.);
#7523=ORIENTED_EDGE('',*,*,#5978,.T.);
#7524=ORIENTED_EDGE('',*,*,#5979,.F.);
#7525=ORIENTED_EDGE('',*,*,#5978,.F.);
#7526=ORIENTED_EDGE('',*,*,#5980,.F.);
#7527=ORIENTED_EDGE('',*,*,#5981,.T.);
#7528=ORIENTED_EDGE('',*,*,#5982,.F.);
#7529=ORIENTED_EDGE('',*,*,#5981,.F.);
#7530=ORIENTED_EDGE('',*,*,#5983,.F.);
#7531=ORIENTED_EDGE('',*,*,#5984,.F.);
#7532=ORIENTED_EDGE('',*,*,#5985,.F.);
#7533=ORIENTED_EDGE('',*,*,#5986,.T.);
#7534=ORIENTED_EDGE('',*,*,#5979,.T.);
#7535=ORIENTED_EDGE('',*,*,#5982,.T.);
#7536=ORIENTED_EDGE('',*,*,#5985,.T.);
#7537=ORIENTED_EDGE('',*,*,#5987,.T.);
#7538=ORIENTED_EDGE('',*,*,#5988,.T.);
#7539=ORIENTED_EDGE('',*,*,#5989,.T.);
#7540=ORIENTED_EDGE('',*,*,#5990,.T.);
#7541=ORIENTED_EDGE('',*,*,#5991,.F.);
#7542=ORIENTED_EDGE('',*,*,#5992,.F.);
#7543=ORIENTED_EDGE('',*,*,#5993,.T.);
#7544=ORIENTED_EDGE('',*,*,#5976,.T.);
#7545=ORIENTED_EDGE('',*,*,#5973,.T.);
#7546=ORIENTED_EDGE('',*,*,#5970,.T.);
#7547=ORIENTED_EDGE('',*,*,#5967,.T.);
#7548=ORIENTED_EDGE('',*,*,#5964,.T.);
#7549=ORIENTED_EDGE('',*,*,#5994,.T.);
#7550=ORIENTED_EDGE('',*,*,#5995,.F.);
#7551=ORIENTED_EDGE('',*,*,#5990,.F.);
#7552=ORIENTED_EDGE('',*,*,#5996,.T.);
#7553=ORIENTED_EDGE('',*,*,#5987,.F.);
#7554=ORIENTED_EDGE('',*,*,#5984,.T.);
#7555=ORIENTED_EDGE('',*,*,#5992,.T.);
#7556=ORIENTED_EDGE('',*,*,#5997,.F.);
#7557=ORIENTED_EDGE('',*,*,#5998,.F.);
#7558=ORIENTED_EDGE('',*,*,#5986,.F.);
#7559=ORIENTED_EDGE('',*,*,#5989,.F.);
#7560=ORIENTED_EDGE('',*,*,#5999,.T.);
#7561=ORIENTED_EDGE('',*,*,#5983,.T.);
#7562=ORIENTED_EDGE('',*,*,#5998,.T.);
#7563=ORIENTED_EDGE('',*,*,#6000,.F.);
#7564=ORIENTED_EDGE('',*,*,#5994,.F.);
#7565=ORIENTED_EDGE('',*,*,#5974,.T.);
#7566=ORIENTED_EDGE('',*,*,#5971,.T.);
#7567=ORIENTED_EDGE('',*,*,#5968,.T.);
#7568=ORIENTED_EDGE('',*,*,#5965,.T.);
#7569=ORIENTED_EDGE('',*,*,#5962,.T.);
#7570=ORIENTED_EDGE('',*,*,#5995,.T.);
#7571=ORIENTED_EDGE('',*,*,#6000,.T.);
#7572=ORIENTED_EDGE('',*,*,#5997,.T.);
#7573=ORIENTED_EDGE('',*,*,#5991,.T.);
#7574=ORIENTED_EDGE('',*,*,#5996,.F.);
#7575=ORIENTED_EDGE('',*,*,#5993,.F.);
#7576=ORIENTED_EDGE('',*,*,#5999,.F.);
#7577=ORIENTED_EDGE('',*,*,#5988,.F.);
#7578=ORIENTED_EDGE('',*,*,#5977,.T.);
#7579=ORIENTED_EDGE('',*,*,#5980,.T.);
#7580=ORIENTED_EDGE('',*,*,#6001,.F.);
#7581=ORIENTED_EDGE('',*,*,#6002,.T.);
#7582=ORIENTED_EDGE('',*,*,#6003,.F.);
#7583=ORIENTED_EDGE('',*,*,#6002,.F.);
#7584=ORIENTED_EDGE('',*,*,#6001,.T.);
#7585=ORIENTED_EDGE('',*,*,#6004,.F.);
#7586=ORIENTED_EDGE('',*,*,#6005,.T.);
#7587=ORIENTED_EDGE('',*,*,#6006,.F.);
#7588=ORIENTED_EDGE('',*,*,#6005,.F.);
#7589=ORIENTED_EDGE('',*,*,#6004,.T.);
#7590=ORIENTED_EDGE('',*,*,#6007,.F.);
#7591=ORIENTED_EDGE('',*,*,#6008,.T.);
#7592=ORIENTED_EDGE('',*,*,#6009,.F.);
#7593=ORIENTED_EDGE('',*,*,#6008,.F.);
#7594=ORIENTED_EDGE('',*,*,#6007,.T.);
#7595=ORIENTED_EDGE('',*,*,#6010,.F.);
#7596=ORIENTED_EDGE('',*,*,#6011,.T.);
#7597=ORIENTED_EDGE('',*,*,#6012,.F.);
#7598=ORIENTED_EDGE('',*,*,#6011,.F.);
#7599=ORIENTED_EDGE('',*,*,#6010,.T.);
#7600=ORIENTED_EDGE('',*,*,#6013,.F.);
#7601=ORIENTED_EDGE('',*,*,#6014,.T.);
#7602=ORIENTED_EDGE('',*,*,#6015,.F.);
#7603=ORIENTED_EDGE('',*,*,#6014,.F.);
#7604=ORIENTED_EDGE('',*,*,#6013,.T.);
#7605=ORIENTED_EDGE('',*,*,#6016,.T.);
#7606=ORIENTED_EDGE('',*,*,#6017,.F.);
#7607=ORIENTED_EDGE('',*,*,#6018,.T.);
#7608=ORIENTED_EDGE('',*,*,#6016,.F.);
#7609=ORIENTED_EDGE('',*,*,#6018,.F.);
#7610=ORIENTED_EDGE('',*,*,#6019,.T.);
#7611=ORIENTED_EDGE('',*,*,#6020,.T.);
#7612=ORIENTED_EDGE('',*,*,#6021,.F.);
#7613=ORIENTED_EDGE('',*,*,#6022,.F.);
#7614=ORIENTED_EDGE('',*,*,#6015,.T.);
#7615=ORIENTED_EDGE('',*,*,#6012,.T.);
#7616=ORIENTED_EDGE('',*,*,#6009,.T.);
#7617=ORIENTED_EDGE('',*,*,#6006,.T.);
#7618=ORIENTED_EDGE('',*,*,#6003,.T.);
#7619=ORIENTED_EDGE('',*,*,#6023,.T.);
#7620=ORIENTED_EDGE('',*,*,#6022,.T.);
#7621=ORIENTED_EDGE('',*,*,#6024,.F.);
#7622=ORIENTED_EDGE('',*,*,#6025,.F.);
#7623=ORIENTED_EDGE('',*,*,#6026,.T.);
#7624=ORIENTED_EDGE('',*,*,#6025,.T.);
#7625=ORIENTED_EDGE('',*,*,#6027,.F.);
#7626=ORIENTED_EDGE('',*,*,#6028,.F.);
#7627=ORIENTED_EDGE('',*,*,#6017,.T.);
#7628=ORIENTED_EDGE('',*,*,#6029,.T.);
#7629=ORIENTED_EDGE('',*,*,#6028,.T.);
#7630=ORIENTED_EDGE('',*,*,#6030,.F.);
#7631=ORIENTED_EDGE('',*,*,#6020,.F.);
#7632=ORIENTED_EDGE('',*,*,#6030,.T.);
#7633=ORIENTED_EDGE('',*,*,#6027,.T.);
#7634=ORIENTED_EDGE('',*,*,#6024,.T.);
#7635=ORIENTED_EDGE('',*,*,#6021,.T.);
#7636=ORIENTED_EDGE('',*,*,#6029,.F.);
#7637=ORIENTED_EDGE('',*,*,#6019,.F.);
#7638=ORIENTED_EDGE('',*,*,#6023,.F.);
#7639=ORIENTED_EDGE('',*,*,#6026,.F.);
#7640=ORIENTED_EDGE('',*,*,#6031,.F.);
#7641=ORIENTED_EDGE('',*,*,#6032,.F.);
#7642=ORIENTED_EDGE('',*,*,#6033,.T.);
#7643=ORIENTED_EDGE('',*,*,#6034,.T.);
#7644=ORIENTED_EDGE('',*,*,#6035,.F.);
#7645=ORIENTED_EDGE('',*,*,#6034,.F.);
#7646=ORIENTED_EDGE('',*,*,#6036,.T.);
#7647=ORIENTED_EDGE('',*,*,#6037,.T.);
#7648=ORIENTED_EDGE('',*,*,#6038,.F.);
#7649=ORIENTED_EDGE('',*,*,#6037,.F.);
#7650=ORIENTED_EDGE('',*,*,#6039,.T.);
#7651=ORIENTED_EDGE('',*,*,#6040,.T.);
#7652=ORIENTED_EDGE('',*,*,#6041,.F.);
#7653=ORIENTED_EDGE('',*,*,#6040,.F.);
#7654=ORIENTED_EDGE('',*,*,#6042,.T.);
#7655=ORIENTED_EDGE('',*,*,#6043,.T.);
#7656=ORIENTED_EDGE('',*,*,#6044,.F.);
#7657=ORIENTED_EDGE('',*,*,#6043,.F.);
#7658=ORIENTED_EDGE('',*,*,#6045,.T.);
#7659=ORIENTED_EDGE('',*,*,#6046,.T.);
#7660=ORIENTED_EDGE('',*,*,#6047,.F.);
#7661=ORIENTED_EDGE('',*,*,#6046,.F.);
#7662=ORIENTED_EDGE('',*,*,#6048,.T.);
#7663=ORIENTED_EDGE('',*,*,#6032,.T.);
#7664=ORIENTED_EDGE('',*,*,#6039,.F.);
#7665=ORIENTED_EDGE('',*,*,#6036,.F.);
#7666=ORIENTED_EDGE('',*,*,#6033,.F.);
#7667=ORIENTED_EDGE('',*,*,#6048,.F.);
#7668=ORIENTED_EDGE('',*,*,#6045,.F.);
#7669=ORIENTED_EDGE('',*,*,#6042,.F.);
#7670=ORIENTED_EDGE('',*,*,#6049,.F.);
#7671=ORIENTED_EDGE('',*,*,#6050,.T.);
#7672=ORIENTED_EDGE('',*,*,#6051,.F.);
#7673=ORIENTED_EDGE('',*,*,#6052,.T.);
#7674=ORIENTED_EDGE('',*,*,#6049,.T.);
#7675=ORIENTED_EDGE('',*,*,#6052,.F.);
#7676=ORIENTED_EDGE('',*,*,#6051,.T.);
#7677=ORIENTED_EDGE('',*,*,#6041,.T.);
#7678=ORIENTED_EDGE('',*,*,#6044,.T.);
#7679=ORIENTED_EDGE('',*,*,#6047,.T.);
#7680=ORIENTED_EDGE('',*,*,#6031,.T.);
#7681=ORIENTED_EDGE('',*,*,#6035,.T.);
#7682=ORIENTED_EDGE('',*,*,#6038,.T.);
#7683=ORIENTED_EDGE('',*,*,#6050,.F.);
#7684=ORIENTED_EDGE('',*,*,#6053,.T.);
#7685=ORIENTED_EDGE('',*,*,#6054,.T.);
#7686=ORIENTED_EDGE('',*,*,#6053,.F.);
#7687=ORIENTED_EDGE('',*,*,#6054,.F.);
#7688=ORIENTED_EDGE('',*,*,#6055,.F.);
#7689=ORIENTED_EDGE('',*,*,#6056,.F.);
#7690=ORIENTED_EDGE('',*,*,#6057,.T.);
#7691=ORIENTED_EDGE('',*,*,#6058,.T.);
#7692=ORIENTED_EDGE('',*,*,#6059,.F.);
#7693=ORIENTED_EDGE('',*,*,#6058,.F.);
#7694=ORIENTED_EDGE('',*,*,#6060,.T.);
#7695=ORIENTED_EDGE('',*,*,#6061,.T.);
#7696=ORIENTED_EDGE('',*,*,#6062,.F.);
#7697=ORIENTED_EDGE('',*,*,#6061,.F.);
#7698=ORIENTED_EDGE('',*,*,#6063,.T.);
#7699=ORIENTED_EDGE('',*,*,#6064,.T.);
#7700=ORIENTED_EDGE('',*,*,#6065,.F.);
#7701=ORIENTED_EDGE('',*,*,#6064,.F.);
#7702=ORIENTED_EDGE('',*,*,#6066,.T.);
#7703=ORIENTED_EDGE('',*,*,#6067,.T.);
#7704=ORIENTED_EDGE('',*,*,#6068,.F.);
#7705=ORIENTED_EDGE('',*,*,#6067,.F.);
#7706=ORIENTED_EDGE('',*,*,#6069,.T.);
#7707=ORIENTED_EDGE('',*,*,#6070,.T.);
#7708=ORIENTED_EDGE('',*,*,#6071,.F.);
#7709=ORIENTED_EDGE('',*,*,#6070,.F.);
#7710=ORIENTED_EDGE('',*,*,#6072,.T.);
#7711=ORIENTED_EDGE('',*,*,#6056,.T.);
#7712=ORIENTED_EDGE('',*,*,#6063,.F.);
#7713=ORIENTED_EDGE('',*,*,#6060,.F.);
#7714=ORIENTED_EDGE('',*,*,#6057,.F.);
#7715=ORIENTED_EDGE('',*,*,#6072,.F.);
#7716=ORIENTED_EDGE('',*,*,#6069,.F.);
#7717=ORIENTED_EDGE('',*,*,#6066,.F.);
#7718=ORIENTED_EDGE('',*,*,#6073,.F.);
#7719=ORIENTED_EDGE('',*,*,#6074,.T.);
#7720=ORIENTED_EDGE('',*,*,#6075,.F.);
#7721=ORIENTED_EDGE('',*,*,#6076,.T.);
#7722=ORIENTED_EDGE('',*,*,#6073,.T.);
#7723=ORIENTED_EDGE('',*,*,#6076,.F.);
#7724=ORIENTED_EDGE('',*,*,#6075,.T.);
#7725=ORIENTED_EDGE('',*,*,#6065,.T.);
#7726=ORIENTED_EDGE('',*,*,#6068,.T.);
#7727=ORIENTED_EDGE('',*,*,#6071,.T.);
#7728=ORIENTED_EDGE('',*,*,#6055,.T.);
#7729=ORIENTED_EDGE('',*,*,#6059,.T.);
#7730=ORIENTED_EDGE('',*,*,#6062,.T.);
#7731=ORIENTED_EDGE('',*,*,#6074,.F.);
#7732=ORIENTED_EDGE('',*,*,#6077,.T.);
#7733=ORIENTED_EDGE('',*,*,#6078,.T.);
#7734=ORIENTED_EDGE('',*,*,#6077,.F.);
#7735=ORIENTED_EDGE('',*,*,#6078,.F.);
#7736=ORIENTED_EDGE('',*,*,#6079,.F.);
#7737=ORIENTED_EDGE('',*,*,#6080,.F.);
#7738=ORIENTED_EDGE('',*,*,#6081,.T.);
#7739=ORIENTED_EDGE('',*,*,#6082,.T.);
#7740=ORIENTED_EDGE('',*,*,#6083,.F.);
#7741=ORIENTED_EDGE('',*,*,#6082,.F.);
#7742=ORIENTED_EDGE('',*,*,#6084,.T.);
#7743=ORIENTED_EDGE('',*,*,#6085,.T.);
#7744=ORIENTED_EDGE('',*,*,#6086,.F.);
#7745=ORIENTED_EDGE('',*,*,#6085,.F.);
#7746=ORIENTED_EDGE('',*,*,#6087,.T.);
#7747=ORIENTED_EDGE('',*,*,#6088,.T.);
#7748=ORIENTED_EDGE('',*,*,#6089,.F.);
#7749=ORIENTED_EDGE('',*,*,#6088,.F.);
#7750=ORIENTED_EDGE('',*,*,#6090,.T.);
#7751=ORIENTED_EDGE('',*,*,#6091,.T.);
#7752=ORIENTED_EDGE('',*,*,#6092,.F.);
#7753=ORIENTED_EDGE('',*,*,#6091,.F.);
#7754=ORIENTED_EDGE('',*,*,#6093,.T.);
#7755=ORIENTED_EDGE('',*,*,#6094,.T.);
#7756=ORIENTED_EDGE('',*,*,#6095,.F.);
#7757=ORIENTED_EDGE('',*,*,#6094,.F.);
#7758=ORIENTED_EDGE('',*,*,#6096,.T.);
#7759=ORIENTED_EDGE('',*,*,#6080,.T.);
#7760=ORIENTED_EDGE('',*,*,#6087,.F.);
#7761=ORIENTED_EDGE('',*,*,#6084,.F.);
#7762=ORIENTED_EDGE('',*,*,#6081,.F.);
#7763=ORIENTED_EDGE('',*,*,#6096,.F.);
#7764=ORIENTED_EDGE('',*,*,#6093,.F.);
#7765=ORIENTED_EDGE('',*,*,#6090,.F.);
#7766=ORIENTED_EDGE('',*,*,#6097,.F.);
#7767=ORIENTED_EDGE('',*,*,#6098,.T.);
#7768=ORIENTED_EDGE('',*,*,#6099,.F.);
#7769=ORIENTED_EDGE('',*,*,#6100,.T.);
#7770=ORIENTED_EDGE('',*,*,#6097,.T.);
#7771=ORIENTED_EDGE('',*,*,#6100,.F.);
#7772=ORIENTED_EDGE('',*,*,#6099,.T.);
#7773=ORIENTED_EDGE('',*,*,#6089,.T.);
#7774=ORIENTED_EDGE('',*,*,#6092,.T.);
#7775=ORIENTED_EDGE('',*,*,#6095,.T.);
#7776=ORIENTED_EDGE('',*,*,#6079,.T.);
#7777=ORIENTED_EDGE('',*,*,#6083,.T.);
#7778=ORIENTED_EDGE('',*,*,#6086,.T.);
#7779=ORIENTED_EDGE('',*,*,#6098,.F.);
#7780=ORIENTED_EDGE('',*,*,#6101,.T.);
#7781=ORIENTED_EDGE('',*,*,#6102,.T.);
#7782=ORIENTED_EDGE('',*,*,#6101,.F.);
#7783=ORIENTED_EDGE('',*,*,#6102,.F.);
#7784=ORIENTED_EDGE('',*,*,#6103,.F.);
#7785=ORIENTED_EDGE('',*,*,#6104,.F.);
#7786=ORIENTED_EDGE('',*,*,#6105,.T.);
#7787=ORIENTED_EDGE('',*,*,#6106,.T.);
#7788=ORIENTED_EDGE('',*,*,#6107,.F.);
#7789=ORIENTED_EDGE('',*,*,#6106,.F.);
#7790=ORIENTED_EDGE('',*,*,#6108,.T.);
#7791=ORIENTED_EDGE('',*,*,#6109,.T.);
#7792=ORIENTED_EDGE('',*,*,#6110,.F.);
#7793=ORIENTED_EDGE('',*,*,#6109,.F.);
#7794=ORIENTED_EDGE('',*,*,#6111,.T.);
#7795=ORIENTED_EDGE('',*,*,#6112,.T.);
#7796=ORIENTED_EDGE('',*,*,#6113,.F.);
#7797=ORIENTED_EDGE('',*,*,#6112,.F.);
#7798=ORIENTED_EDGE('',*,*,#6114,.T.);
#7799=ORIENTED_EDGE('',*,*,#6115,.T.);
#7800=ORIENTED_EDGE('',*,*,#6116,.F.);
#7801=ORIENTED_EDGE('',*,*,#6115,.F.);
#7802=ORIENTED_EDGE('',*,*,#6117,.T.);
#7803=ORIENTED_EDGE('',*,*,#6118,.T.);
#7804=ORIENTED_EDGE('',*,*,#6119,.F.);
#7805=ORIENTED_EDGE('',*,*,#6118,.F.);
#7806=ORIENTED_EDGE('',*,*,#6120,.T.);
#7807=ORIENTED_EDGE('',*,*,#6104,.T.);
#7808=ORIENTED_EDGE('',*,*,#6111,.F.);
#7809=ORIENTED_EDGE('',*,*,#6108,.F.);
#7810=ORIENTED_EDGE('',*,*,#6105,.F.);
#7811=ORIENTED_EDGE('',*,*,#6120,.F.);
#7812=ORIENTED_EDGE('',*,*,#6117,.F.);
#7813=ORIENTED_EDGE('',*,*,#6114,.F.);
#7814=ORIENTED_EDGE('',*,*,#6121,.F.);
#7815=ORIENTED_EDGE('',*,*,#6122,.T.);
#7816=ORIENTED_EDGE('',*,*,#6123,.F.);
#7817=ORIENTED_EDGE('',*,*,#6124,.T.);
#7818=ORIENTED_EDGE('',*,*,#6121,.T.);
#7819=ORIENTED_EDGE('',*,*,#6124,.F.);
#7820=ORIENTED_EDGE('',*,*,#6123,.T.);
#7821=ORIENTED_EDGE('',*,*,#6113,.T.);
#7822=ORIENTED_EDGE('',*,*,#6116,.T.);
#7823=ORIENTED_EDGE('',*,*,#6119,.T.);
#7824=ORIENTED_EDGE('',*,*,#6103,.T.);
#7825=ORIENTED_EDGE('',*,*,#6107,.T.);
#7826=ORIENTED_EDGE('',*,*,#6110,.T.);
#7827=ORIENTED_EDGE('',*,*,#6122,.F.);
#7828=ORIENTED_EDGE('',*,*,#6125,.T.);
#7829=ORIENTED_EDGE('',*,*,#6126,.T.);
#7830=ORIENTED_EDGE('',*,*,#6125,.F.);
#7831=ORIENTED_EDGE('',*,*,#6126,.F.);
#7832=ORIENTED_EDGE('',*,*,#6127,.F.);
#7833=ORIENTED_EDGE('',*,*,#6128,.F.);
#7834=ORIENTED_EDGE('',*,*,#6129,.F.);
#7835=ORIENTED_EDGE('',*,*,#6130,.T.);
#7836=ORIENTED_EDGE('',*,*,#6131,.F.);
#7837=ORIENTED_EDGE('',*,*,#6132,.F.);
#7838=ORIENTED_EDGE('',*,*,#6133,.T.);
#7839=ORIENTED_EDGE('',*,*,#6134,.F.);
#7840=ORIENTED_EDGE('',*,*,#6133,.F.);
#7841=ORIENTED_EDGE('',*,*,#6135,.F.);
#7842=ORIENTED_EDGE('',*,*,#6136,.F.);
#7843=ORIENTED_EDGE('',*,*,#6137,.T.);
#7844=ORIENTED_EDGE('',*,*,#6138,.F.);
#7845=ORIENTED_EDGE('',*,*,#6139,.F.);
#7846=ORIENTED_EDGE('',*,*,#6128,.T.);
#7847=ORIENTED_EDGE('',*,*,#6140,.F.);
#7848=ORIENTED_EDGE('',*,*,#6141,.F.);
#7849=ORIENTED_EDGE('',*,*,#6137,.F.);
#7850=ORIENTED_EDGE('',*,*,#6142,.F.);
#7851=ORIENTED_EDGE('',*,*,#6130,.F.);
#7852=ORIENTED_EDGE('',*,*,#6135,.T.);
#7853=ORIENTED_EDGE('',*,*,#6132,.T.);
#7854=ORIENTED_EDGE('',*,*,#6143,.F.);
#7855=ORIENTED_EDGE('',*,*,#6144,.T.);
#7856=ORIENTED_EDGE('',*,*,#6145,.F.);
#7857=ORIENTED_EDGE('',*,*,#6146,.T.);
#7858=ORIENTED_EDGE('',*,*,#6146,.F.);
#7859=ORIENTED_EDGE('',*,*,#6136,.T.);
#7860=ORIENTED_EDGE('',*,*,#6134,.T.);
#7861=ORIENTED_EDGE('',*,*,#6147,.F.);
#7862=ORIENTED_EDGE('',*,*,#6148,.T.);
#7863=ORIENTED_EDGE('',*,*,#6149,.F.);
#7864=ORIENTED_EDGE('',*,*,#6150,.F.);
#7865=ORIENTED_EDGE('',*,*,#6151,.F.);
#7866=ORIENTED_EDGE('',*,*,#6152,.T.);
#7867=ORIENTED_EDGE('',*,*,#6153,.F.);
#7868=ORIENTED_EDGE('',*,*,#6154,.F.);
#7869=ORIENTED_EDGE('',*,*,#6155,.T.);
#7870=ORIENTED_EDGE('',*,*,#6156,.F.);
#7871=ORIENTED_EDGE('',*,*,#6155,.F.);
#7872=ORIENTED_EDGE('',*,*,#6157,.F.);
#7873=ORIENTED_EDGE('',*,*,#6148,.F.);
#7874=ORIENTED_EDGE('',*,*,#6158,.F.);
#7875=ORIENTED_EDGE('',*,*,#6159,.T.);
#7876=ORIENTED_EDGE('',*,*,#6160,.F.);
#7877=ORIENTED_EDGE('',*,*,#6161,.F.);
#7878=ORIENTED_EDGE('',*,*,#6152,.F.);
#7879=ORIENTED_EDGE('',*,*,#6162,.F.);
#7880=ORIENTED_EDGE('',*,*,#6159,.F.);
#7881=ORIENTED_EDGE('',*,*,#6163,.T.);
#7882=ORIENTED_EDGE('',*,*,#6164,.T.);
#7883=ORIENTED_EDGE('',*,*,#6165,.T.);
#7884=ORIENTED_EDGE('',*,*,#6166,.T.);
#7885=ORIENTED_EDGE('',*,*,#6129,.T.);
#7886=ORIENTED_EDGE('',*,*,#6145,.T.);
#7887=ORIENTED_EDGE('',*,*,#6167,.T.);
#7888=ORIENTED_EDGE('',*,*,#6153,.T.);
#7889=ORIENTED_EDGE('',*,*,#6156,.T.);
#7890=ORIENTED_EDGE('',*,*,#6147,.T.);
#7891=ORIENTED_EDGE('',*,*,#6168,.T.);
#7892=ORIENTED_EDGE('',*,*,#6169,.T.);
#7893=ORIENTED_EDGE('',*,*,#6140,.T.);
#7894=ORIENTED_EDGE('',*,*,#6127,.T.);
#7895=ORIENTED_EDGE('',*,*,#6139,.T.);
#7896=ORIENTED_EDGE('',*,*,#6170,.T.);
#7897=ORIENTED_EDGE('',*,*,#6171,.T.);
#7898=ORIENTED_EDGE('',*,*,#6150,.T.);
#7899=ORIENTED_EDGE('',*,*,#6161,.T.);
#7900=ORIENTED_EDGE('',*,*,#6158,.T.);
#7901=ORIENTED_EDGE('',*,*,#6172,.T.);
#7902=ORIENTED_EDGE('',*,*,#6143,.T.);
#7903=ORIENTED_EDGE('',*,*,#6131,.T.);
#7904=ORIENTED_EDGE('',*,*,#6142,.T.);
#7905=ORIENTED_EDGE('',*,*,#6173,.T.);
#7906=ORIENTED_EDGE('',*,*,#6174,.T.);
#7907=ORIENTED_EDGE('',*,*,#6175,.F.);
#7908=ORIENTED_EDGE('',*,*,#6176,.F.);
#7909=ORIENTED_EDGE('',*,*,#6177,.F.);
#7910=ORIENTED_EDGE('',*,*,#6178,.F.);
#7911=ORIENTED_EDGE('',*,*,#6151,.T.);
#7912=ORIENTED_EDGE('',*,*,#6171,.F.);
#7913=ORIENTED_EDGE('',*,*,#6179,.F.);
#7914=ORIENTED_EDGE('',*,*,#6168,.F.);
#7915=ORIENTED_EDGE('',*,*,#6149,.T.);
#7916=ORIENTED_EDGE('',*,*,#6157,.T.);
#7917=ORIENTED_EDGE('',*,*,#6154,.T.);
#7918=ORIENTED_EDGE('',*,*,#6167,.F.);
#7919=ORIENTED_EDGE('',*,*,#6144,.F.);
#7920=ORIENTED_EDGE('',*,*,#6172,.F.);
#7921=ORIENTED_EDGE('',*,*,#6160,.T.);
#7922=ORIENTED_EDGE('',*,*,#6162,.T.);
#7923=ORIENTED_EDGE('',*,*,#6138,.T.);
#7924=ORIENTED_EDGE('',*,*,#6141,.T.);
#7925=ORIENTED_EDGE('',*,*,#6169,.F.);
#7926=ORIENTED_EDGE('',*,*,#6179,.T.);
#7927=ORIENTED_EDGE('',*,*,#6170,.F.);
#7928=ORIENTED_EDGE('',*,*,#6177,.T.);
#7929=ORIENTED_EDGE('',*,*,#6180,.T.);
#7930=ORIENTED_EDGE('',*,*,#6181,.F.);
#7931=ORIENTED_EDGE('',*,*,#6182,.F.);
#7932=ORIENTED_EDGE('',*,*,#6183,.T.);
#7933=ORIENTED_EDGE('',*,*,#6184,.T.);
#7934=ORIENTED_EDGE('',*,*,#6176,.T.);
#7935=ORIENTED_EDGE('',*,*,#6185,.F.);
#7936=ORIENTED_EDGE('',*,*,#6186,.F.);
#7937=ORIENTED_EDGE('',*,*,#6180,.F.);
#7938=ORIENTED_EDGE('',*,*,#6187,.F.);
#7939=ORIENTED_EDGE('',*,*,#6188,.T.);
#7940=ORIENTED_EDGE('',*,*,#6189,.T.);
#7941=ORIENTED_EDGE('',*,*,#6183,.F.);
#7942=ORIENTED_EDGE('',*,*,#6175,.T.);
#7943=ORIENTED_EDGE('',*,*,#6190,.T.);
#7944=ORIENTED_EDGE('',*,*,#6188,.F.);
#7945=ORIENTED_EDGE('',*,*,#6191,.F.);
#7946=ORIENTED_EDGE('',*,*,#6192,.T.);
#7947=ORIENTED_EDGE('',*,*,#6185,.T.);
#7948=ORIENTED_EDGE('',*,*,#6193,.F.);
#7949=ORIENTED_EDGE('',*,*,#6181,.T.);
#7950=ORIENTED_EDGE('',*,*,#6186,.T.);
#7951=ORIENTED_EDGE('',*,*,#6192,.F.);
#7952=ORIENTED_EDGE('',*,*,#6178,.T.);
#7953=ORIENTED_EDGE('',*,*,#6184,.F.);
#7954=ORIENTED_EDGE('',*,*,#6189,.F.);
#7955=ORIENTED_EDGE('',*,*,#6190,.F.);
#7956=ORIENTED_EDGE('',*,*,#6194,.F.);
#7957=ORIENTED_EDGE('',*,*,#6195,.T.);
#7958=ORIENTED_EDGE('',*,*,#6174,.F.);
#7959=ORIENTED_EDGE('',*,*,#6195,.F.);
#7960=ORIENTED_EDGE('',*,*,#6196,.F.);
#7961=ORIENTED_EDGE('',*,*,#6197,.T.);
#7962=ORIENTED_EDGE('',*,*,#6173,.F.);
#7963=ORIENTED_EDGE('',*,*,#6197,.F.);
#7964=ORIENTED_EDGE('',*,*,#6198,.T.);
#7965=ORIENTED_EDGE('',*,*,#6199,.T.);
#7966=ORIENTED_EDGE('',*,*,#6166,.F.);
#7967=ORIENTED_EDGE('',*,*,#6200,.F.);
#7968=ORIENTED_EDGE('',*,*,#6201,.T.);
#7969=ORIENTED_EDGE('',*,*,#6200,.T.);
#7970=ORIENTED_EDGE('',*,*,#6165,.F.);
#7971=ORIENTED_EDGE('',*,*,#6202,.F.);
#7972=ORIENTED_EDGE('',*,*,#6203,.T.);
#7973=ORIENTED_EDGE('',*,*,#6202,.T.);
#7974=ORIENTED_EDGE('',*,*,#6164,.F.);
#7975=ORIENTED_EDGE('',*,*,#6204,.F.);
#7976=ORIENTED_EDGE('',*,*,#6205,.T.);
#7977=ORIENTED_EDGE('',*,*,#6204,.T.);
#7978=ORIENTED_EDGE('',*,*,#6163,.F.);
#7979=ORIENTED_EDGE('',*,*,#6199,.F.);
#7980=ORIENTED_EDGE('',*,*,#6205,.F.);
#7981=ORIENTED_EDGE('',*,*,#6198,.F.);
#7982=ORIENTED_EDGE('',*,*,#6201,.F.);
#7983=ORIENTED_EDGE('',*,*,#6203,.F.);
#7984=ORIENTED_EDGE('',*,*,#6182,.T.);
#7985=ORIENTED_EDGE('',*,*,#6193,.T.);
#7986=ORIENTED_EDGE('',*,*,#6191,.T.);
#7987=ORIENTED_EDGE('',*,*,#6187,.T.);
#7988=ORIENTED_EDGE('',*,*,#6194,.T.);
#7989=ORIENTED_EDGE('',*,*,#6196,.T.);
#7990=ORIENTED_EDGE('',*,*,#6206,.T.);
#7991=ORIENTED_EDGE('',*,*,#6207,.T.);
#7992=ORIENTED_EDGE('',*,*,#6208,.F.);
#7993=ORIENTED_EDGE('',*,*,#6207,.F.);
#7994=ORIENTED_EDGE('',*,*,#6209,.F.);
#7995=ORIENTED_EDGE('',*,*,#6208,.T.);
#7996=ORIENTED_EDGE('',*,*,#6210,.T.);
#7997=ORIENTED_EDGE('',*,*,#6210,.F.);
#7998=ORIENTED_EDGE('',*,*,#6209,.T.);
#7999=ORIENTED_EDGE('',*,*,#6211,.F.);
#8000=ORIENTED_EDGE('',*,*,#6211,.T.);
#8001=ORIENTED_EDGE('',*,*,#6206,.F.);
#8002=ORIENTED_EDGE('',*,*,#6212,.F.);
#8003=ORIENTED_EDGE('',*,*,#6213,.F.);
#8004=ORIENTED_EDGE('',*,*,#6214,.F.);
#8005=ORIENTED_EDGE('',*,*,#6215,.T.);
#8006=ORIENTED_EDGE('',*,*,#6216,.F.);
#8007=ORIENTED_EDGE('',*,*,#6215,.F.);
#8008=ORIENTED_EDGE('',*,*,#6217,.F.);
#8009=ORIENTED_EDGE('',*,*,#6218,.T.);
#8010=ORIENTED_EDGE('',*,*,#6219,.F.);
#8011=ORIENTED_EDGE('',*,*,#6220,.F.);
#8012=ORIENTED_EDGE('',*,*,#6221,.F.);
#8013=ORIENTED_EDGE('',*,*,#6218,.F.);
#8014=ORIENTED_EDGE('',*,*,#6222,.F.);
#8015=ORIENTED_EDGE('',*,*,#6223,.T.);
#8016=ORIENTED_EDGE('',*,*,#6224,.T.);
#8017=ORIENTED_EDGE('',*,*,#6223,.F.);
#8018=ORIENTED_EDGE('',*,*,#6213,.T.);
#8019=ORIENTED_EDGE('',*,*,#6212,.T.);
#8020=ORIENTED_EDGE('',*,*,#6214,.T.);
#8021=ORIENTED_EDGE('',*,*,#6220,.T.);
#8022=ORIENTED_EDGE('',*,*,#6219,.T.);
#8023=ORIENTED_EDGE('',*,*,#6221,.T.);
#8024=ORIENTED_EDGE('',*,*,#6225,.T.);
#8025=ORIENTED_EDGE('',*,*,#6226,.T.);
#8026=ORIENTED_EDGE('',*,*,#6227,.T.);
#8027=ORIENTED_EDGE('',*,*,#6228,.T.);
#8028=ORIENTED_EDGE('',*,*,#6229,.T.);
#8029=ORIENTED_EDGE('',*,*,#6230,.T.);
#8030=ORIENTED_EDGE('',*,*,#6231,.T.);
#8031=ORIENTED_EDGE('',*,*,#6232,.T.);
#8032=ORIENTED_EDGE('',*,*,#6233,.T.);
#8033=ORIENTED_EDGE('',*,*,#6234,.T.);
#8034=ORIENTED_EDGE('',*,*,#6235,.T.);
#8035=ORIENTED_EDGE('',*,*,#6236,.T.);
#8036=ORIENTED_EDGE('',*,*,#6226,.F.);
#8037=ORIENTED_EDGE('',*,*,#6225,.F.);
#8038=ORIENTED_EDGE('',*,*,#6227,.F.);
#8039=ORIENTED_EDGE('',*,*,#6237,.T.);
#8040=ORIENTED_EDGE('',*,*,#6238,.F.);
#8041=ORIENTED_EDGE('',*,*,#6237,.F.);
#8042=ORIENTED_EDGE('',*,*,#6239,.F.);
#8043=ORIENTED_EDGE('',*,*,#6240,.T.);
#8044=ORIENTED_EDGE('',*,*,#6229,.F.);
#8045=ORIENTED_EDGE('',*,*,#6228,.F.);
#8046=ORIENTED_EDGE('',*,*,#6230,.F.);
#8047=ORIENTED_EDGE('',*,*,#6240,.F.);
#8048=ORIENTED_EDGE('',*,*,#6232,.F.);
#8049=ORIENTED_EDGE('',*,*,#6231,.F.);
#8050=ORIENTED_EDGE('',*,*,#6233,.F.);
#8051=ORIENTED_EDGE('',*,*,#6241,.T.);
#8052=ORIENTED_EDGE('',*,*,#6242,.F.);
#8053=ORIENTED_EDGE('',*,*,#6241,.F.);
#8054=ORIENTED_EDGE('',*,*,#6243,.F.);
#8055=ORIENTED_EDGE('',*,*,#6244,.T.);
#8056=ORIENTED_EDGE('',*,*,#6235,.F.);
#8057=ORIENTED_EDGE('',*,*,#6234,.F.);
#8058=ORIENTED_EDGE('',*,*,#6236,.F.);
#8059=ORIENTED_EDGE('',*,*,#6244,.F.);
#8060=ORIENTED_EDGE('',*,*,#6224,.F.);
#8061=ORIENTED_EDGE('',*,*,#6245,.T.);
#8062=ORIENTED_EDGE('',*,*,#6246,.F.);
#8063=ORIENTED_EDGE('',*,*,#6222,.T.);
#8064=ORIENTED_EDGE('',*,*,#6247,.F.);
#8065=ORIENTED_EDGE('',*,*,#6248,.T.);
#8066=ORIENTED_EDGE('',*,*,#6246,.T.);
#8067=ORIENTED_EDGE('',*,*,#6248,.F.);
#8068=ORIENTED_EDGE('',*,*,#6247,.T.);
#8069=ORIENTED_EDGE('',*,*,#6249,.F.);
#8070=ORIENTED_EDGE('',*,*,#6249,.T.);
#8071=ORIENTED_EDGE('',*,*,#6250,.T.);
#8072=ORIENTED_EDGE('',*,*,#6245,.F.);
#8073=ORIENTED_EDGE('',*,*,#6250,.F.);
#8074=ORIENTED_EDGE('',*,*,#6217,.T.);
#8075=ORIENTED_EDGE('',*,*,#6216,.T.);
#8076=ORIENTED_EDGE('',*,*,#6239,.T.);
#8077=ORIENTED_EDGE('',*,*,#6238,.T.);
#8078=ORIENTED_EDGE('',*,*,#6243,.T.);
#8079=ORIENTED_EDGE('',*,*,#6242,.T.);
#8080=ORIENTED_EDGE('',*,*,#6251,.F.);
#8081=ORIENTED_EDGE('',*,*,#6252,.T.);
#8082=ORIENTED_EDGE('',*,*,#6253,.T.);
#8083=ORIENTED_EDGE('',*,*,#6252,.F.);
#8084=ORIENTED_EDGE('',*,*,#6254,.F.);
#8085=ORIENTED_EDGE('',*,*,#6255,.T.);
#8086=ORIENTED_EDGE('',*,*,#6256,.T.);
#8087=ORIENTED_EDGE('',*,*,#6255,.F.);
#8088=ORIENTED_EDGE('',*,*,#6254,.T.);
#8089=ORIENTED_EDGE('',*,*,#6251,.T.);
#8090=ORIENTED_EDGE('',*,*,#6256,.F.);
#8091=ORIENTED_EDGE('',*,*,#6253,.F.);
#8092=ORIENTED_EDGE('',*,*,#6257,.T.);
#8093=ORIENTED_EDGE('',*,*,#6258,.T.);
#8094=ORIENTED_EDGE('',*,*,#6259,.T.);
#8095=ORIENTED_EDGE('',*,*,#6260,.F.);
#8096=ORIENTED_EDGE('',*,*,#6261,.T.);
#8097=ORIENTED_EDGE('',*,*,#6262,.T.);
#8098=ORIENTED_EDGE('',*,*,#6263,.T.);
#8099=ORIENTED_EDGE('',*,*,#6258,.F.);
#8100=ORIENTED_EDGE('',*,*,#6264,.T.);
#8101=ORIENTED_EDGE('',*,*,#6265,.T.);
#8102=ORIENTED_EDGE('',*,*,#6266,.T.);
#8103=ORIENTED_EDGE('',*,*,#6262,.F.);
#8104=ORIENTED_EDGE('',*,*,#6267,.T.);
#8105=ORIENTED_EDGE('',*,*,#6268,.T.);
#8106=ORIENTED_EDGE('',*,*,#6269,.T.);
#8107=ORIENTED_EDGE('',*,*,#6265,.F.);
#8108=ORIENTED_EDGE('',*,*,#6270,.T.);
#8109=ORIENTED_EDGE('',*,*,#6271,.T.);
#8110=ORIENTED_EDGE('',*,*,#6272,.T.);
#8111=ORIENTED_EDGE('',*,*,#6268,.F.);
#8112=ORIENTED_EDGE('',*,*,#6273,.T.);
#8113=ORIENTED_EDGE('',*,*,#6260,.T.);
#8114=ORIENTED_EDGE('',*,*,#6274,.T.);
#8115=ORIENTED_EDGE('',*,*,#6271,.F.);
#8116=ORIENTED_EDGE('',*,*,#6273,.F.);
#8117=ORIENTED_EDGE('',*,*,#6270,.F.);
#8118=ORIENTED_EDGE('',*,*,#6267,.F.);
#8119=ORIENTED_EDGE('',*,*,#6264,.F.);
#8120=ORIENTED_EDGE('',*,*,#6261,.F.);
#8121=ORIENTED_EDGE('',*,*,#6257,.F.);
#8122=ORIENTED_EDGE('',*,*,#6274,.F.);
#8123=ORIENTED_EDGE('',*,*,#6259,.F.);
#8124=ORIENTED_EDGE('',*,*,#6263,.F.);
#8125=ORIENTED_EDGE('',*,*,#6266,.F.);
#8126=ORIENTED_EDGE('',*,*,#6269,.F.);
#8127=ORIENTED_EDGE('',*,*,#6272,.F.);
#8128=ORIENTED_EDGE('',*,*,#6275,.F.);
#8129=ORIENTED_EDGE('',*,*,#6276,.F.);
#8130=ORIENTED_EDGE('',*,*,#6277,.F.);
#8131=ORIENTED_EDGE('',*,*,#6278,.T.);
#8132=ORIENTED_EDGE('',*,*,#6276,.T.);
#8133=ORIENTED_EDGE('',*,*,#6278,.F.);
#8134=ORIENTED_EDGE('',*,*,#6279,.F.);
#8135=ORIENTED_EDGE('',*,*,#6280,.T.);
#8136=ORIENTED_EDGE('',*,*,#6277,.T.);
#8137=ORIENTED_EDGE('',*,*,#6280,.F.);
#8138=ORIENTED_EDGE('',*,*,#6281,.F.);
#8139=ORIENTED_EDGE('',*,*,#6282,.T.);
#8140=ORIENTED_EDGE('',*,*,#6279,.T.);
#8141=ORIENTED_EDGE('',*,*,#6282,.F.);
#8142=ORIENTED_EDGE('',*,*,#6281,.T.);
#8143=ORIENTED_EDGE('',*,*,#6283,.F.);
#8144=ORIENTED_EDGE('',*,*,#6284,.F.);
#8145=ORIENTED_EDGE('',*,*,#6285,.T.);
#8146=ORIENTED_EDGE('',*,*,#6283,.T.);
#8147=ORIENTED_EDGE('',*,*,#6285,.F.);
#8148=ORIENTED_EDGE('',*,*,#6275,.T.);
#8149=ORIENTED_EDGE('',*,*,#6286,.T.);
#8150=ORIENTED_EDGE('',*,*,#6284,.T.);
#8151=ORIENTED_EDGE('',*,*,#6286,.F.);
#8152=ORIENTED_EDGE('',*,*,#6287,.T.);
#8153=ORIENTED_EDGE('',*,*,#6288,.T.);
#8154=ORIENTED_EDGE('',*,*,#6289,.T.);
#8155=ORIENTED_EDGE('',*,*,#6290,.F.);
#8156=ORIENTED_EDGE('',*,*,#6291,.T.);
#8157=ORIENTED_EDGE('',*,*,#6292,.T.);
#8158=ORIENTED_EDGE('',*,*,#6293,.T.);
#8159=ORIENTED_EDGE('',*,*,#6288,.F.);
#8160=ORIENTED_EDGE('',*,*,#6294,.T.);
#8161=ORIENTED_EDGE('',*,*,#6295,.T.);
#8162=ORIENTED_EDGE('',*,*,#6296,.T.);
#8163=ORIENTED_EDGE('',*,*,#6292,.F.);
#8164=ORIENTED_EDGE('',*,*,#6297,.T.);
#8165=ORIENTED_EDGE('',*,*,#6298,.T.);
#8166=ORIENTED_EDGE('',*,*,#6299,.T.);
#8167=ORIENTED_EDGE('',*,*,#6295,.F.);
#8168=ORIENTED_EDGE('',*,*,#6300,.T.);
#8169=ORIENTED_EDGE('',*,*,#6301,.T.);
#8170=ORIENTED_EDGE('',*,*,#6302,.T.);
#8171=ORIENTED_EDGE('',*,*,#6298,.F.);
#8172=ORIENTED_EDGE('',*,*,#6303,.T.);
#8173=ORIENTED_EDGE('',*,*,#6290,.T.);
#8174=ORIENTED_EDGE('',*,*,#6304,.T.);
#8175=ORIENTED_EDGE('',*,*,#6301,.F.);
#8176=ORIENTED_EDGE('',*,*,#6303,.F.);
#8177=ORIENTED_EDGE('',*,*,#6300,.F.);
#8178=ORIENTED_EDGE('',*,*,#6297,.F.);
#8179=ORIENTED_EDGE('',*,*,#6294,.F.);
#8180=ORIENTED_EDGE('',*,*,#6291,.F.);
#8181=ORIENTED_EDGE('',*,*,#6287,.F.);
#8182=ORIENTED_EDGE('',*,*,#6304,.F.);
#8183=ORIENTED_EDGE('',*,*,#6289,.F.);
#8184=ORIENTED_EDGE('',*,*,#6293,.F.);
#8185=ORIENTED_EDGE('',*,*,#6296,.F.);
#8186=ORIENTED_EDGE('',*,*,#6299,.F.);
#8187=ORIENTED_EDGE('',*,*,#6302,.F.);
#8188=ORIENTED_EDGE('',*,*,#6305,.F.);
#8189=ORIENTED_EDGE('',*,*,#6306,.F.);
#8190=ORIENTED_EDGE('',*,*,#6307,.F.);
#8191=ORIENTED_EDGE('',*,*,#6308,.T.);
#8192=ORIENTED_EDGE('',*,*,#6306,.T.);
#8193=ORIENTED_EDGE('',*,*,#6308,.F.);
#8194=ORIENTED_EDGE('',*,*,#6309,.F.);
#8195=ORIENTED_EDGE('',*,*,#6310,.T.);
#8196=ORIENTED_EDGE('',*,*,#6307,.T.);
#8197=ORIENTED_EDGE('',*,*,#6310,.F.);
#8198=ORIENTED_EDGE('',*,*,#6311,.F.);
#8199=ORIENTED_EDGE('',*,*,#6312,.T.);
#8200=ORIENTED_EDGE('',*,*,#6309,.T.);
#8201=ORIENTED_EDGE('',*,*,#6312,.F.);
#8202=ORIENTED_EDGE('',*,*,#6311,.T.);
#8203=ORIENTED_EDGE('',*,*,#6313,.F.);
#8204=ORIENTED_EDGE('',*,*,#6314,.F.);
#8205=ORIENTED_EDGE('',*,*,#6315,.T.);
#8206=ORIENTED_EDGE('',*,*,#6313,.T.);
#8207=ORIENTED_EDGE('',*,*,#6315,.F.);
#8208=ORIENTED_EDGE('',*,*,#6305,.T.);
#8209=ORIENTED_EDGE('',*,*,#6316,.T.);
#8210=ORIENTED_EDGE('',*,*,#6314,.T.);
#8211=ORIENTED_EDGE('',*,*,#6316,.F.);
#8212=ORIENTED_EDGE('',*,*,#6317,.F.);
#8213=ORIENTED_EDGE('',*,*,#6318,.T.);
#8214=ORIENTED_EDGE('',*,*,#6319,.F.);
#8215=ORIENTED_EDGE('',*,*,#6320,.T.);
#8216=ORIENTED_EDGE('',*,*,#6321,.F.);
#8217=ORIENTED_EDGE('',*,*,#6320,.F.);
#8218=ORIENTED_EDGE('',*,*,#6322,.F.);
#8219=ORIENTED_EDGE('',*,*,#6323,.F.);
#8220=ORIENTED_EDGE('',*,*,#6324,.F.);
#8221=ORIENTED_EDGE('',*,*,#6323,.T.);
#8222=ORIENTED_EDGE('',*,*,#6325,.T.);
#8223=ORIENTED_EDGE('',*,*,#6326,.T.);
#8224=ORIENTED_EDGE('',*,*,#6322,.T.);
#8225=ORIENTED_EDGE('',*,*,#6319,.T.);
#8226=ORIENTED_EDGE('',*,*,#6327,.T.);
#8227=ORIENTED_EDGE('',*,*,#6325,.F.);
#8228=ORIENTED_EDGE('',*,*,#6328,.F.);
#8229=ORIENTED_EDGE('',*,*,#6326,.F.);
#8230=ORIENTED_EDGE('',*,*,#6327,.F.);
#8231=ORIENTED_EDGE('',*,*,#6318,.F.);
#8232=ORIENTED_EDGE('',*,*,#6329,.F.);
#8233=ORIENTED_EDGE('',*,*,#6330,.T.);
#8234=ORIENTED_EDGE('',*,*,#6331,.F.);
#8235=ORIENTED_EDGE('',*,*,#6330,.F.);
#8236=ORIENTED_EDGE('',*,*,#6329,.T.);
#8237=ORIENTED_EDGE('',*,*,#6332,.F.);
#8238=ORIENTED_EDGE('',*,*,#6333,.T.);
#8239=ORIENTED_EDGE('',*,*,#6334,.T.);
#8240=ORIENTED_EDGE('',*,*,#6333,.F.);
#8241=ORIENTED_EDGE('',*,*,#6324,.T.);
#8242=ORIENTED_EDGE('',*,*,#6328,.T.);
#8243=ORIENTED_EDGE('',*,*,#6317,.T.);
#8244=ORIENTED_EDGE('',*,*,#6321,.T.);
#8245=ORIENTED_EDGE('',*,*,#6332,.T.);
#8246=ORIENTED_EDGE('',*,*,#6331,.T.);
#8247=ORIENTED_EDGE('',*,*,#6334,.F.);
#8248=ORIENTED_EDGE('',*,*,#6335,.F.);
#8249=ORIENTED_EDGE('',*,*,#6336,.T.);
#8250=ORIENTED_EDGE('',*,*,#6337,.T.);
#8251=ORIENTED_EDGE('',*,*,#6336,.F.);
#8252=ORIENTED_EDGE('',*,*,#6335,.T.);
#8253=ORIENTED_EDGE('',*,*,#6337,.F.);
#8254=ORIENTED_EDGE('',*,*,#6338,.F.);
#8255=ORIENTED_EDGE('',*,*,#6339,.T.);
#8256=ORIENTED_EDGE('',*,*,#6340,.F.);
#8257=ORIENTED_EDGE('',*,*,#6341,.F.);
#8258=ORIENTED_EDGE('',*,*,#6342,.T.);
#8259=ORIENTED_EDGE('',*,*,#6343,.F.);
#8260=ORIENTED_EDGE('',*,*,#6344,.F.);
#8261=ORIENTED_EDGE('',*,*,#6342,.F.);
#8262=ORIENTED_EDGE('',*,*,#6345,.F.);
#8263=ORIENTED_EDGE('',*,*,#6346,.F.);
#8264=ORIENTED_EDGE('',*,*,#6339,.F.);
#8265=ORIENTED_EDGE('',*,*,#6347,.F.);
#8266=ORIENTED_EDGE('',*,*,#6345,.T.);
#8267=ORIENTED_EDGE('',*,*,#6341,.T.);
#8268=ORIENTED_EDGE('',*,*,#6348,.F.);
#8269=ORIENTED_EDGE('',*,*,#6349,.T.);
#8270=ORIENTED_EDGE('',*,*,#6350,.T.);
#8271=ORIENTED_EDGE('',*,*,#6349,.F.);
#8272=ORIENTED_EDGE('',*,*,#6346,.T.);
#8273=ORIENTED_EDGE('',*,*,#6347,.T.);
#8274=ORIENTED_EDGE('',*,*,#6340,.T.);
#8275=ORIENTED_EDGE('',*,*,#6338,.T.);
#8276=ORIENTED_EDGE('',*,*,#6351,.F.);
#8277=ORIENTED_EDGE('',*,*,#6352,.T.);
#8278=ORIENTED_EDGE('',*,*,#6353,.T.);
#8279=ORIENTED_EDGE('',*,*,#6352,.F.);
#8280=ORIENTED_EDGE('',*,*,#6343,.T.);
#8281=ORIENTED_EDGE('',*,*,#6344,.T.);
#8282=ORIENTED_EDGE('',*,*,#6351,.T.);
#8283=ORIENTED_EDGE('',*,*,#6348,.T.);
#8284=ORIENTED_EDGE('',*,*,#6353,.F.);
#8285=ORIENTED_EDGE('',*,*,#6350,.F.);
#8286=ORIENTED_EDGE('',*,*,#6354,.F.);
#8287=ORIENTED_EDGE('',*,*,#6355,.T.);
#8288=ORIENTED_EDGE('',*,*,#6356,.F.);
#8289=ORIENTED_EDGE('',*,*,#6357,.F.);
#8290=ORIENTED_EDGE('',*,*,#6358,.T.);
#8291=ORIENTED_EDGE('',*,*,#6359,.F.);
#8292=ORIENTED_EDGE('',*,*,#6360,.F.);
#8293=ORIENTED_EDGE('',*,*,#6358,.F.);
#8294=ORIENTED_EDGE('',*,*,#6361,.F.);
#8295=ORIENTED_EDGE('',*,*,#6362,.F.);
#8296=ORIENTED_EDGE('',*,*,#6355,.F.);
#8297=ORIENTED_EDGE('',*,*,#6363,.F.);
#8298=ORIENTED_EDGE('',*,*,#6361,.T.);
#8299=ORIENTED_EDGE('',*,*,#6357,.T.);
#8300=ORIENTED_EDGE('',*,*,#6364,.F.);
#8301=ORIENTED_EDGE('',*,*,#6365,.T.);
#8302=ORIENTED_EDGE('',*,*,#6366,.F.);
#8303=ORIENTED_EDGE('',*,*,#6367,.F.);
#8304=ORIENTED_EDGE('',*,*,#6368,.F.);
#8305=ORIENTED_EDGE('',*,*,#6369,.T.);
#8306=ORIENTED_EDGE('',*,*,#6370,.F.);
#8307=ORIENTED_EDGE('',*,*,#6365,.F.);
#8308=ORIENTED_EDGE('',*,*,#6371,.F.);
#8309=ORIENTED_EDGE('',*,*,#6372,.F.);
#8310=ORIENTED_EDGE('',*,*,#6373,.F.);
#8311=ORIENTED_EDGE('',*,*,#6369,.F.);
#8312=ORIENTED_EDGE('',*,*,#6374,.T.);
#8313=ORIENTED_EDGE('',*,*,#6366,.T.);
#8314=ORIENTED_EDGE('',*,*,#6370,.T.);
#8315=ORIENTED_EDGE('',*,*,#6373,.T.);
#8316=ORIENTED_EDGE('',*,*,#6375,.T.);
#8317=ORIENTED_EDGE('',*,*,#6367,.T.);
#8318=ORIENTED_EDGE('',*,*,#6375,.F.);
#8319=ORIENTED_EDGE('',*,*,#6372,.T.);
#8320=ORIENTED_EDGE('',*,*,#6376,.T.);
#8321=ORIENTED_EDGE('',*,*,#6362,.T.);
#8322=ORIENTED_EDGE('',*,*,#6363,.T.);
#8323=ORIENTED_EDGE('',*,*,#6356,.T.);
#8324=ORIENTED_EDGE('',*,*,#6354,.T.);
#8325=ORIENTED_EDGE('',*,*,#6377,.T.);
#8326=ORIENTED_EDGE('',*,*,#6378,.F.);
#8327=ORIENTED_EDGE('',*,*,#6379,.F.);
#8328=ORIENTED_EDGE('',*,*,#6380,.F.);
#8329=ORIENTED_EDGE('',*,*,#6377,.F.);
#8330=ORIENTED_EDGE('',*,*,#6381,.T.);
#8331=ORIENTED_EDGE('',*,*,#6379,.T.);
#8332=ORIENTED_EDGE('',*,*,#6381,.F.);
#8333=ORIENTED_EDGE('',*,*,#6380,.T.);
#8334=ORIENTED_EDGE('',*,*,#6382,.T.);
#8335=ORIENTED_EDGE('',*,*,#6383,.T.);
#8336=ORIENTED_EDGE('',*,*,#6382,.F.);
#8337=ORIENTED_EDGE('',*,*,#6359,.T.);
#8338=ORIENTED_EDGE('',*,*,#6360,.T.);
#8339=ORIENTED_EDGE('',*,*,#6374,.F.);
#8340=ORIENTED_EDGE('',*,*,#6384,.T.);
#8341=ORIENTED_EDGE('',*,*,#6378,.T.);
#8342=ORIENTED_EDGE('',*,*,#6384,.F.);
#8343=ORIENTED_EDGE('',*,*,#6383,.F.);
#8344=ORIENTED_EDGE('',*,*,#6364,.T.);
#8345=ORIENTED_EDGE('',*,*,#6376,.F.);
#8346=ORIENTED_EDGE('',*,*,#6371,.T.);
#8347=ORIENTED_EDGE('',*,*,#6368,.T.);
#8348=ORIENTED_EDGE('',*,*,#6385,.F.);
#8349=ORIENTED_EDGE('',*,*,#6386,.T.);
#8350=ORIENTED_EDGE('',*,*,#6387,.F.);
#8351=ORIENTED_EDGE('',*,*,#6388,.F.);
#8352=ORIENTED_EDGE('',*,*,#6389,.T.);
#8353=ORIENTED_EDGE('',*,*,#6390,.F.);
#8354=ORIENTED_EDGE('',*,*,#6391,.F.);
#8355=ORIENTED_EDGE('',*,*,#6389,.F.);
#8356=ORIENTED_EDGE('',*,*,#6392,.F.);
#8357=ORIENTED_EDGE('',*,*,#6393,.F.);
#8358=ORIENTED_EDGE('',*,*,#6386,.F.);
#8359=ORIENTED_EDGE('',*,*,#6394,.F.);
#8360=ORIENTED_EDGE('',*,*,#6392,.T.);
#8361=ORIENTED_EDGE('',*,*,#6388,.T.);
#8362=ORIENTED_EDGE('',*,*,#6395,.F.);
#8363=ORIENTED_EDGE('',*,*,#6396,.T.);
#8364=ORIENTED_EDGE('',*,*,#6397,.T.);
#8365=ORIENTED_EDGE('',*,*,#6396,.F.);
#8366=ORIENTED_EDGE('',*,*,#6393,.T.);
#8367=ORIENTED_EDGE('',*,*,#6394,.T.);
#8368=ORIENTED_EDGE('',*,*,#6387,.T.);
#8369=ORIENTED_EDGE('',*,*,#6385,.T.);
#8370=ORIENTED_EDGE('',*,*,#6398,.F.);
#8371=ORIENTED_EDGE('',*,*,#6399,.T.);
#8372=ORIENTED_EDGE('',*,*,#6400,.T.);
#8373=ORIENTED_EDGE('',*,*,#6399,.F.);
#8374=ORIENTED_EDGE('',*,*,#6390,.T.);
#8375=ORIENTED_EDGE('',*,*,#6391,.T.);
#8376=ORIENTED_EDGE('',*,*,#6398,.T.);
#8377=ORIENTED_EDGE('',*,*,#6395,.T.);
#8378=ORIENTED_EDGE('',*,*,#6400,.F.);
#8379=ORIENTED_EDGE('',*,*,#6397,.F.);
#8380=ORIENTED_EDGE('',*,*,#6401,.F.);
#8381=ORIENTED_EDGE('',*,*,#6402,.T.);
#8382=ORIENTED_EDGE('',*,*,#6403,.F.);
#8383=ORIENTED_EDGE('',*,*,#6404,.F.);
#8384=ORIENTED_EDGE('',*,*,#6405,.T.);
#8385=ORIENTED_EDGE('',*,*,#6406,.F.);
#8386=ORIENTED_EDGE('',*,*,#6407,.F.);
#8387=ORIENTED_EDGE('',*,*,#6405,.F.);
#8388=ORIENTED_EDGE('',*,*,#6408,.F.);
#8389=ORIENTED_EDGE('',*,*,#6409,.F.);
#8390=ORIENTED_EDGE('',*,*,#6402,.F.);
#8391=ORIENTED_EDGE('',*,*,#6410,.F.);
#8392=ORIENTED_EDGE('',*,*,#6408,.T.);
#8393=ORIENTED_EDGE('',*,*,#6404,.T.);
#8394=ORIENTED_EDGE('',*,*,#6411,.F.);
#8395=ORIENTED_EDGE('',*,*,#6412,.T.);
#8396=ORIENTED_EDGE('',*,*,#6413,.T.);
#8397=ORIENTED_EDGE('',*,*,#6412,.F.);
#8398=ORIENTED_EDGE('',*,*,#6409,.T.);
#8399=ORIENTED_EDGE('',*,*,#6410,.T.);
#8400=ORIENTED_EDGE('',*,*,#6403,.T.);
#8401=ORIENTED_EDGE('',*,*,#6401,.T.);
#8402=ORIENTED_EDGE('',*,*,#6414,.F.);
#8403=ORIENTED_EDGE('',*,*,#6415,.T.);
#8404=ORIENTED_EDGE('',*,*,#6416,.T.);
#8405=ORIENTED_EDGE('',*,*,#6415,.F.);
#8406=ORIENTED_EDGE('',*,*,#6406,.T.);
#8407=ORIENTED_EDGE('',*,*,#6407,.T.);
#8408=ORIENTED_EDGE('',*,*,#6414,.T.);
#8409=ORIENTED_EDGE('',*,*,#6411,.T.);
#8410=ORIENTED_EDGE('',*,*,#6416,.F.);
#8411=ORIENTED_EDGE('',*,*,#6413,.F.);
#8412=ORIENTED_EDGE('',*,*,#6417,.F.);
#8413=ORIENTED_EDGE('',*,*,#6418,.T.);
#8414=ORIENTED_EDGE('',*,*,#6419,.T.);
#8415=ORIENTED_EDGE('',*,*,#6418,.F.);
#8416=ORIENTED_EDGE('',*,*,#6420,.F.);
#8417=ORIENTED_EDGE('',*,*,#6421,.T.);
#8418=ORIENTED_EDGE('',*,*,#6422,.T.);
#8419=ORIENTED_EDGE('',*,*,#6421,.F.);
#8420=ORIENTED_EDGE('',*,*,#6420,.T.);
#8421=ORIENTED_EDGE('',*,*,#6417,.T.);
#8422=ORIENTED_EDGE('',*,*,#6422,.F.);
#8423=ORIENTED_EDGE('',*,*,#6419,.F.);
#8424=ORIENTED_EDGE('',*,*,#6423,.F.);
#8425=ORIENTED_EDGE('',*,*,#6424,.T.);
#8426=ORIENTED_EDGE('',*,*,#6425,.T.);
#8427=ORIENTED_EDGE('',*,*,#6426,.F.);
#8428=ORIENTED_EDGE('',*,*,#6427,.F.);
#8429=ORIENTED_EDGE('',*,*,#6428,.T.);
#8430=ORIENTED_EDGE('',*,*,#6429,.T.);
#8431=ORIENTED_EDGE('',*,*,#6424,.F.);
#8432=ORIENTED_EDGE('',*,*,#6430,.F.);
#8433=ORIENTED_EDGE('',*,*,#6431,.T.);
#8434=ORIENTED_EDGE('',*,*,#6432,.T.);
#8435=ORIENTED_EDGE('',*,*,#6428,.F.);
#8436=ORIENTED_EDGE('',*,*,#6433,.F.);
#8437=ORIENTED_EDGE('',*,*,#6434,.T.);
#8438=ORIENTED_EDGE('',*,*,#6435,.T.);
#8439=ORIENTED_EDGE('',*,*,#6431,.F.);
#8440=ORIENTED_EDGE('',*,*,#6436,.F.);
#8441=ORIENTED_EDGE('',*,*,#6437,.T.);
#8442=ORIENTED_EDGE('',*,*,#6438,.T.);
#8443=ORIENTED_EDGE('',*,*,#6434,.F.);
#8444=ORIENTED_EDGE('',*,*,#6439,.F.);
#8445=ORIENTED_EDGE('',*,*,#6426,.T.);
#8446=ORIENTED_EDGE('',*,*,#6440,.T.);
#8447=ORIENTED_EDGE('',*,*,#6437,.F.);
#8448=ORIENTED_EDGE('',*,*,#6440,.F.);
#8449=ORIENTED_EDGE('',*,*,#6425,.F.);
#8450=ORIENTED_EDGE('',*,*,#6429,.F.);
#8451=ORIENTED_EDGE('',*,*,#6432,.F.);
#8452=ORIENTED_EDGE('',*,*,#6435,.F.);
#8453=ORIENTED_EDGE('',*,*,#6438,.F.);
#8454=ORIENTED_EDGE('',*,*,#6441,.F.);
#8455=ORIENTED_EDGE('',*,*,#6423,.T.);
#8456=ORIENTED_EDGE('',*,*,#6439,.T.);
#8457=ORIENTED_EDGE('',*,*,#6436,.T.);
#8458=ORIENTED_EDGE('',*,*,#6433,.T.);
#8459=ORIENTED_EDGE('',*,*,#6430,.T.);
#8460=ORIENTED_EDGE('',*,*,#6427,.T.);
#8461=ORIENTED_EDGE('',*,*,#6442,.F.);
#8462=ORIENTED_EDGE('',*,*,#6443,.T.);
#8463=ORIENTED_EDGE('',*,*,#6441,.T.);
#8464=ORIENTED_EDGE('',*,*,#6443,.F.);
#8465=ORIENTED_EDGE('',*,*,#6444,.F.);
#8466=ORIENTED_EDGE('',*,*,#6445,.T.);
#8467=ORIENTED_EDGE('',*,*,#6442,.T.);
#8468=ORIENTED_EDGE('',*,*,#6445,.F.);
#8469=ORIENTED_EDGE('',*,*,#6446,.F.);
#8470=ORIENTED_EDGE('',*,*,#6447,.T.);
#8471=ORIENTED_EDGE('',*,*,#6444,.T.);
#8472=ORIENTED_EDGE('',*,*,#6447,.F.);
#8473=ORIENTED_EDGE('',*,*,#6446,.T.);
#8474=ORIENTED_EDGE('',*,*,#6448,.F.);
#8475=ORIENTED_EDGE('',*,*,#6449,.F.);
#8476=ORIENTED_EDGE('',*,*,#6450,.T.);
#8477=ORIENTED_EDGE('',*,*,#6451,.F.);
#8478=ORIENTED_EDGE('',*,*,#6450,.F.);
#8479=ORIENTED_EDGE('',*,*,#6452,.F.);
#8480=ORIENTED_EDGE('',*,*,#6453,.T.);
#8481=ORIENTED_EDGE('',*,*,#6454,.F.);
#8482=ORIENTED_EDGE('',*,*,#6453,.F.);
#8483=ORIENTED_EDGE('',*,*,#6448,.T.);
#8484=ORIENTED_EDGE('',*,*,#6449,.T.);
#8485=ORIENTED_EDGE('',*,*,#6455,.F.);
#8486=ORIENTED_EDGE('',*,*,#6456,.T.);
#8487=ORIENTED_EDGE('',*,*,#6457,.F.);
#8488=ORIENTED_EDGE('',*,*,#6458,.F.);
#8489=ORIENTED_EDGE('',*,*,#6459,.F.);
#8490=ORIENTED_EDGE('',*,*,#6458,.T.);
#8491=ORIENTED_EDGE('',*,*,#6460,.F.);
#8492=ORIENTED_EDGE('',*,*,#6461,.F.);
#8493=ORIENTED_EDGE('',*,*,#6462,.F.);
#8494=ORIENTED_EDGE('',*,*,#6461,.T.);
#8495=ORIENTED_EDGE('',*,*,#6463,.F.);
#8496=ORIENTED_EDGE('',*,*,#6464,.F.);
#8497=ORIENTED_EDGE('',*,*,#6465,.F.);
#8498=ORIENTED_EDGE('',*,*,#6464,.T.);
#8499=ORIENTED_EDGE('',*,*,#6466,.F.);
#8500=ORIENTED_EDGE('',*,*,#6467,.F.);
#8501=ORIENTED_EDGE('',*,*,#6468,.F.);
#8502=ORIENTED_EDGE('',*,*,#6467,.T.);
#8503=ORIENTED_EDGE('',*,*,#6469,.F.);
#8504=ORIENTED_EDGE('',*,*,#6470,.F.);
#8505=ORIENTED_EDGE('',*,*,#6471,.F.);
#8506=ORIENTED_EDGE('',*,*,#6470,.T.);
#8507=ORIENTED_EDGE('',*,*,#6472,.F.);
#8508=ORIENTED_EDGE('',*,*,#6473,.F.);
#8509=ORIENTED_EDGE('',*,*,#6474,.F.);
#8510=ORIENTED_EDGE('',*,*,#6473,.T.);
#8511=ORIENTED_EDGE('',*,*,#6475,.F.);
#8512=ORIENTED_EDGE('',*,*,#6476,.F.);
#8513=ORIENTED_EDGE('',*,*,#6477,.F.);
#8514=ORIENTED_EDGE('',*,*,#6476,.T.);
#8515=ORIENTED_EDGE('',*,*,#6478,.F.);
#8516=ORIENTED_EDGE('',*,*,#6479,.F.);
#8517=ORIENTED_EDGE('',*,*,#6480,.F.);
#8518=ORIENTED_EDGE('',*,*,#6479,.T.);
#8519=ORIENTED_EDGE('',*,*,#6481,.F.);
#8520=ORIENTED_EDGE('',*,*,#6482,.F.);
#8521=ORIENTED_EDGE('',*,*,#6483,.F.);
#8522=ORIENTED_EDGE('',*,*,#6482,.T.);
#8523=ORIENTED_EDGE('',*,*,#6484,.F.);
#8524=ORIENTED_EDGE('',*,*,#6485,.F.);
#8525=ORIENTED_EDGE('',*,*,#6486,.F.);
#8526=ORIENTED_EDGE('',*,*,#6485,.T.);
#8527=ORIENTED_EDGE('',*,*,#6487,.F.);
#8528=ORIENTED_EDGE('',*,*,#6488,.F.);
#8529=ORIENTED_EDGE('',*,*,#6489,.F.);
#8530=ORIENTED_EDGE('',*,*,#6488,.T.);
#8531=ORIENTED_EDGE('',*,*,#6490,.F.);
#8532=ORIENTED_EDGE('',*,*,#6491,.F.);
#8533=ORIENTED_EDGE('',*,*,#6492,.F.);
#8534=ORIENTED_EDGE('',*,*,#6491,.T.);
#8535=ORIENTED_EDGE('',*,*,#6493,.F.);
#8536=ORIENTED_EDGE('',*,*,#6494,.F.);
#8537=ORIENTED_EDGE('',*,*,#6495,.F.);
#8538=ORIENTED_EDGE('',*,*,#6494,.T.);
#8539=ORIENTED_EDGE('',*,*,#6496,.F.);
#8540=ORIENTED_EDGE('',*,*,#6497,.F.);
#8541=ORIENTED_EDGE('',*,*,#6498,.F.);
#8542=ORIENTED_EDGE('',*,*,#6497,.T.);
#8543=ORIENTED_EDGE('',*,*,#6499,.F.);
#8544=ORIENTED_EDGE('',*,*,#6500,.F.);
#8545=ORIENTED_EDGE('',*,*,#6501,.F.);
#8546=ORIENTED_EDGE('',*,*,#6500,.T.);
#8547=ORIENTED_EDGE('',*,*,#6502,.F.);
#8548=ORIENTED_EDGE('',*,*,#6503,.F.);
#8549=ORIENTED_EDGE('',*,*,#6504,.F.);
#8550=ORIENTED_EDGE('',*,*,#6503,.T.);
#8551=ORIENTED_EDGE('',*,*,#6505,.F.);
#8552=ORIENTED_EDGE('',*,*,#6506,.F.);
#8553=ORIENTED_EDGE('',*,*,#6507,.F.);
#8554=ORIENTED_EDGE('',*,*,#6506,.T.);
#8555=ORIENTED_EDGE('',*,*,#6508,.F.);
#8556=ORIENTED_EDGE('',*,*,#6456,.F.);
#8557=ORIENTED_EDGE('',*,*,#6507,.T.);
#8558=ORIENTED_EDGE('',*,*,#6455,.T.);
#8559=ORIENTED_EDGE('',*,*,#6459,.T.);
#8560=ORIENTED_EDGE('',*,*,#6462,.T.);
#8561=ORIENTED_EDGE('',*,*,#6465,.T.);
#8562=ORIENTED_EDGE('',*,*,#6468,.T.);
#8563=ORIENTED_EDGE('',*,*,#6471,.T.);
#8564=ORIENTED_EDGE('',*,*,#6474,.T.);
#8565=ORIENTED_EDGE('',*,*,#6477,.T.);
#8566=ORIENTED_EDGE('',*,*,#6480,.T.);
#8567=ORIENTED_EDGE('',*,*,#6483,.T.);
#8568=ORIENTED_EDGE('',*,*,#6486,.T.);
#8569=ORIENTED_EDGE('',*,*,#6489,.T.);
#8570=ORIENTED_EDGE('',*,*,#6492,.T.);
#8571=ORIENTED_EDGE('',*,*,#6495,.T.);
#8572=ORIENTED_EDGE('',*,*,#6498,.T.);
#8573=ORIENTED_EDGE('',*,*,#6501,.T.);
#8574=ORIENTED_EDGE('',*,*,#6504,.T.);
#8575=ORIENTED_EDGE('',*,*,#6457,.T.);
#8576=ORIENTED_EDGE('',*,*,#6509,.T.);
#8577=ORIENTED_EDGE('',*,*,#6460,.T.);
#8578=ORIENTED_EDGE('',*,*,#6510,.T.);
#8579=ORIENTED_EDGE('',*,*,#6463,.T.);
#8580=ORIENTED_EDGE('',*,*,#6511,.T.);
#8581=ORIENTED_EDGE('',*,*,#6466,.T.);
#8582=ORIENTED_EDGE('',*,*,#6512,.T.);
#8583=ORIENTED_EDGE('',*,*,#6469,.T.);
#8584=ORIENTED_EDGE('',*,*,#6513,.T.);
#8585=ORIENTED_EDGE('',*,*,#6472,.T.);
#8586=ORIENTED_EDGE('',*,*,#6514,.T.);
#8587=ORIENTED_EDGE('',*,*,#6475,.T.);
#8588=ORIENTED_EDGE('',*,*,#6515,.T.);
#8589=ORIENTED_EDGE('',*,*,#6478,.T.);
#8590=ORIENTED_EDGE('',*,*,#6516,.T.);
#8591=ORIENTED_EDGE('',*,*,#6481,.T.);
#8592=ORIENTED_EDGE('',*,*,#6517,.T.);
#8593=ORIENTED_EDGE('',*,*,#6518,.T.);
#8594=ORIENTED_EDGE('',*,*,#6519,.T.);
#8595=ORIENTED_EDGE('',*,*,#6520,.T.);
#8596=ORIENTED_EDGE('',*,*,#6521,.T.);
#8597=ORIENTED_EDGE('',*,*,#6522,.T.);
#8598=ORIENTED_EDGE('',*,*,#6523,.T.);
#8599=ORIENTED_EDGE('',*,*,#6524,.T.);
#8600=ORIENTED_EDGE('',*,*,#6525,.T.);
#8601=ORIENTED_EDGE('',*,*,#6526,.T.);
#8602=ORIENTED_EDGE('',*,*,#6527,.T.);
#8603=ORIENTED_EDGE('',*,*,#6528,.T.);
#8604=ORIENTED_EDGE('',*,*,#6529,.T.);
#8605=ORIENTED_EDGE('',*,*,#6530,.T.);
#8606=ORIENTED_EDGE('',*,*,#6531,.T.);
#8607=ORIENTED_EDGE('',*,*,#6532,.T.);
#8608=ORIENTED_EDGE('',*,*,#6533,.T.);
#8609=ORIENTED_EDGE('',*,*,#6534,.T.);
#8610=ORIENTED_EDGE('',*,*,#6535,.T.);
#8611=ORIENTED_EDGE('',*,*,#6536,.T.);
#8612=ORIENTED_EDGE('',*,*,#6537,.T.);
#8613=ORIENTED_EDGE('',*,*,#6538,.T.);
#8614=ORIENTED_EDGE('',*,*,#6539,.T.);
#8615=ORIENTED_EDGE('',*,*,#6540,.T.);
#8616=ORIENTED_EDGE('',*,*,#6508,.T.);
#8617=ORIENTED_EDGE('',*,*,#6505,.T.);
#8618=ORIENTED_EDGE('',*,*,#6502,.T.);
#8619=ORIENTED_EDGE('',*,*,#6499,.T.);
#8620=ORIENTED_EDGE('',*,*,#6496,.T.);
#8621=ORIENTED_EDGE('',*,*,#6493,.T.);
#8622=ORIENTED_EDGE('',*,*,#6490,.T.);
#8623=ORIENTED_EDGE('',*,*,#6487,.T.);
#8624=ORIENTED_EDGE('',*,*,#6484,.T.);
#8625=ORIENTED_EDGE('',*,*,#6454,.T.);
#8626=ORIENTED_EDGE('',*,*,#6541,.F.);
#8627=ORIENTED_EDGE('',*,*,#6542,.T.);
#8628=ORIENTED_EDGE('',*,*,#6543,.F.);
#8629=ORIENTED_EDGE('',*,*,#6544,.F.);
#8630=ORIENTED_EDGE('',*,*,#6545,.F.);
#8631=ORIENTED_EDGE('',*,*,#6544,.T.);
#8632=ORIENTED_EDGE('',*,*,#6546,.F.);
#8633=ORIENTED_EDGE('',*,*,#6547,.F.);
#8634=ORIENTED_EDGE('',*,*,#6548,.F.);
#8635=ORIENTED_EDGE('',*,*,#6547,.T.);
#8636=ORIENTED_EDGE('',*,*,#6549,.F.);
#8637=ORIENTED_EDGE('',*,*,#6550,.F.);
#8638=ORIENTED_EDGE('',*,*,#6551,.F.);
#8639=ORIENTED_EDGE('',*,*,#6550,.T.);
#8640=ORIENTED_EDGE('',*,*,#6552,.F.);
#8641=ORIENTED_EDGE('',*,*,#6553,.F.);
#8642=ORIENTED_EDGE('',*,*,#6554,.F.);
#8643=ORIENTED_EDGE('',*,*,#6553,.T.);
#8644=ORIENTED_EDGE('',*,*,#6555,.F.);
#8645=ORIENTED_EDGE('',*,*,#6556,.F.);
#8646=ORIENTED_EDGE('',*,*,#6557,.F.);
#8647=ORIENTED_EDGE('',*,*,#6556,.T.);
#8648=ORIENTED_EDGE('',*,*,#6558,.F.);
#8649=ORIENTED_EDGE('',*,*,#6559,.F.);
#8650=ORIENTED_EDGE('',*,*,#6560,.F.);
#8651=ORIENTED_EDGE('',*,*,#6559,.T.);
#8652=ORIENTED_EDGE('',*,*,#6561,.F.);
#8653=ORIENTED_EDGE('',*,*,#6562,.F.);
#8654=ORIENTED_EDGE('',*,*,#6563,.F.);
#8655=ORIENTED_EDGE('',*,*,#6562,.T.);
#8656=ORIENTED_EDGE('',*,*,#6564,.F.);
#8657=ORIENTED_EDGE('',*,*,#6565,.F.);
#8658=ORIENTED_EDGE('',*,*,#6566,.F.);
#8659=ORIENTED_EDGE('',*,*,#6565,.T.);
#8660=ORIENTED_EDGE('',*,*,#6538,.F.);
#8661=ORIENTED_EDGE('',*,*,#6567,.F.);
#8662=ORIENTED_EDGE('',*,*,#6568,.F.);
#8663=ORIENTED_EDGE('',*,*,#6567,.T.);
#8664=ORIENTED_EDGE('',*,*,#6537,.F.);
#8665=ORIENTED_EDGE('',*,*,#6569,.F.);
#8666=ORIENTED_EDGE('',*,*,#6570,.F.);
#8667=ORIENTED_EDGE('',*,*,#6569,.T.);
#8668=ORIENTED_EDGE('',*,*,#6536,.F.);
#8669=ORIENTED_EDGE('',*,*,#6571,.F.);
#8670=ORIENTED_EDGE('',*,*,#6572,.F.);
#8671=ORIENTED_EDGE('',*,*,#6571,.T.);
#8672=ORIENTED_EDGE('',*,*,#6535,.F.);
#8673=ORIENTED_EDGE('',*,*,#6573,.F.);
#8674=ORIENTED_EDGE('',*,*,#6574,.F.);
#8675=ORIENTED_EDGE('',*,*,#6573,.T.);
#8676=ORIENTED_EDGE('',*,*,#6534,.F.);
#8677=ORIENTED_EDGE('',*,*,#6575,.F.);
#8678=ORIENTED_EDGE('',*,*,#6576,.F.);
#8679=ORIENTED_EDGE('',*,*,#6575,.T.);
#8680=ORIENTED_EDGE('',*,*,#6533,.F.);
#8681=ORIENTED_EDGE('',*,*,#6577,.F.);
#8682=ORIENTED_EDGE('',*,*,#6578,.F.);
#8683=ORIENTED_EDGE('',*,*,#6577,.T.);
#8684=ORIENTED_EDGE('',*,*,#6532,.F.);
#8685=ORIENTED_EDGE('',*,*,#6579,.F.);
#8686=ORIENTED_EDGE('',*,*,#6580,.F.);
#8687=ORIENTED_EDGE('',*,*,#6579,.T.);
#8688=ORIENTED_EDGE('',*,*,#6531,.F.);
#8689=ORIENTED_EDGE('',*,*,#6581,.F.);
#8690=ORIENTED_EDGE('',*,*,#6582,.F.);
#8691=ORIENTED_EDGE('',*,*,#6581,.T.);
#8692=ORIENTED_EDGE('',*,*,#6530,.F.);
#8693=ORIENTED_EDGE('',*,*,#6583,.F.);
#8694=ORIENTED_EDGE('',*,*,#6584,.F.);
#8695=ORIENTED_EDGE('',*,*,#6583,.T.);
#8696=ORIENTED_EDGE('',*,*,#6529,.F.);
#8697=ORIENTED_EDGE('',*,*,#6542,.F.);
#8698=ORIENTED_EDGE('',*,*,#6584,.T.);
#8699=ORIENTED_EDGE('',*,*,#6541,.T.);
#8700=ORIENTED_EDGE('',*,*,#6545,.T.);
#8701=ORIENTED_EDGE('',*,*,#6548,.T.);
#8702=ORIENTED_EDGE('',*,*,#6551,.T.);
#8703=ORIENTED_EDGE('',*,*,#6554,.T.);
#8704=ORIENTED_EDGE('',*,*,#6557,.T.);
#8705=ORIENTED_EDGE('',*,*,#6560,.T.);
#8706=ORIENTED_EDGE('',*,*,#6563,.T.);
#8707=ORIENTED_EDGE('',*,*,#6566,.T.);
#8708=ORIENTED_EDGE('',*,*,#6568,.T.);
#8709=ORIENTED_EDGE('',*,*,#6570,.T.);
#8710=ORIENTED_EDGE('',*,*,#6572,.T.);
#8711=ORIENTED_EDGE('',*,*,#6574,.T.);
#8712=ORIENTED_EDGE('',*,*,#6576,.T.);
#8713=ORIENTED_EDGE('',*,*,#6578,.T.);
#8714=ORIENTED_EDGE('',*,*,#6580,.T.);
#8715=ORIENTED_EDGE('',*,*,#6582,.T.);
#8716=ORIENTED_EDGE('',*,*,#6543,.T.);
#8717=ORIENTED_EDGE('',*,*,#6585,.T.);
#8718=ORIENTED_EDGE('',*,*,#6546,.T.);
#8719=ORIENTED_EDGE('',*,*,#6586,.T.);
#8720=ORIENTED_EDGE('',*,*,#6549,.T.);
#8721=ORIENTED_EDGE('',*,*,#6587,.T.);
#8722=ORIENTED_EDGE('',*,*,#6552,.T.);
#8723=ORIENTED_EDGE('',*,*,#6588,.T.);
#8724=ORIENTED_EDGE('',*,*,#6555,.T.);
#8725=ORIENTED_EDGE('',*,*,#6589,.T.);
#8726=ORIENTED_EDGE('',*,*,#6558,.T.);
#8727=ORIENTED_EDGE('',*,*,#6590,.T.);
#8728=ORIENTED_EDGE('',*,*,#6561,.T.);
#8729=ORIENTED_EDGE('',*,*,#6591,.T.);
#8730=ORIENTED_EDGE('',*,*,#6564,.T.);
#8731=ORIENTED_EDGE('',*,*,#6592,.T.);
#8732=ORIENTED_EDGE('',*,*,#6593,.F.);
#8733=ORIENTED_EDGE('',*,*,#6594,.T.);
#8734=ORIENTED_EDGE('',*,*,#6595,.F.);
#8735=ORIENTED_EDGE('',*,*,#6596,.F.);
#8736=ORIENTED_EDGE('',*,*,#6597,.F.);
#8737=ORIENTED_EDGE('',*,*,#6596,.T.);
#8738=ORIENTED_EDGE('',*,*,#6598,.F.);
#8739=ORIENTED_EDGE('',*,*,#6599,.F.);
#8740=ORIENTED_EDGE('',*,*,#6600,.F.);
#8741=ORIENTED_EDGE('',*,*,#6599,.T.);
#8742=ORIENTED_EDGE('',*,*,#6601,.F.);
#8743=ORIENTED_EDGE('',*,*,#6602,.F.);
#8744=ORIENTED_EDGE('',*,*,#6603,.F.);
#8745=ORIENTED_EDGE('',*,*,#6602,.T.);
#8746=ORIENTED_EDGE('',*,*,#6604,.F.);
#8747=ORIENTED_EDGE('',*,*,#6605,.F.);
#8748=ORIENTED_EDGE('',*,*,#6606,.F.);
#8749=ORIENTED_EDGE('',*,*,#6605,.T.);
#8750=ORIENTED_EDGE('',*,*,#6607,.F.);
#8751=ORIENTED_EDGE('',*,*,#6608,.F.);
#8752=ORIENTED_EDGE('',*,*,#6609,.F.);
#8753=ORIENTED_EDGE('',*,*,#6608,.T.);
#8754=ORIENTED_EDGE('',*,*,#6610,.F.);
#8755=ORIENTED_EDGE('',*,*,#6611,.F.);
#8756=ORIENTED_EDGE('',*,*,#6612,.F.);
#8757=ORIENTED_EDGE('',*,*,#6611,.T.);
#8758=ORIENTED_EDGE('',*,*,#6613,.F.);
#8759=ORIENTED_EDGE('',*,*,#6614,.F.);
#8760=ORIENTED_EDGE('',*,*,#6615,.F.);
#8761=ORIENTED_EDGE('',*,*,#6614,.T.);
#8762=ORIENTED_EDGE('',*,*,#6616,.F.);
#8763=ORIENTED_EDGE('',*,*,#6617,.F.);
#8764=ORIENTED_EDGE('',*,*,#6618,.F.);
#8765=ORIENTED_EDGE('',*,*,#6617,.T.);
#8766=ORIENTED_EDGE('',*,*,#6527,.F.);
#8767=ORIENTED_EDGE('',*,*,#6619,.F.);
#8768=ORIENTED_EDGE('',*,*,#6620,.F.);
#8769=ORIENTED_EDGE('',*,*,#6619,.T.);
#8770=ORIENTED_EDGE('',*,*,#6526,.F.);
#8771=ORIENTED_EDGE('',*,*,#6621,.F.);
#8772=ORIENTED_EDGE('',*,*,#6622,.F.);
#8773=ORIENTED_EDGE('',*,*,#6621,.T.);
#8774=ORIENTED_EDGE('',*,*,#6525,.F.);
#8775=ORIENTED_EDGE('',*,*,#6623,.F.);
#8776=ORIENTED_EDGE('',*,*,#6624,.F.);
#8777=ORIENTED_EDGE('',*,*,#6623,.T.);
#8778=ORIENTED_EDGE('',*,*,#6524,.F.);
#8779=ORIENTED_EDGE('',*,*,#6625,.F.);
#8780=ORIENTED_EDGE('',*,*,#6626,.F.);
#8781=ORIENTED_EDGE('',*,*,#6625,.T.);
#8782=ORIENTED_EDGE('',*,*,#6523,.F.);
#8783=ORIENTED_EDGE('',*,*,#6627,.F.);
#8784=ORIENTED_EDGE('',*,*,#6628,.F.);
#8785=ORIENTED_EDGE('',*,*,#6627,.T.);
#8786=ORIENTED_EDGE('',*,*,#6522,.F.);
#8787=ORIENTED_EDGE('',*,*,#6629,.F.);
#8788=ORIENTED_EDGE('',*,*,#6630,.F.);
#8789=ORIENTED_EDGE('',*,*,#6629,.T.);
#8790=ORIENTED_EDGE('',*,*,#6521,.F.);
#8791=ORIENTED_EDGE('',*,*,#6631,.F.);
#8792=ORIENTED_EDGE('',*,*,#6632,.F.);
#8793=ORIENTED_EDGE('',*,*,#6631,.T.);
#8794=ORIENTED_EDGE('',*,*,#6520,.F.);
#8795=ORIENTED_EDGE('',*,*,#6633,.F.);
#8796=ORIENTED_EDGE('',*,*,#6634,.F.);
#8797=ORIENTED_EDGE('',*,*,#6633,.T.);
#8798=ORIENTED_EDGE('',*,*,#6519,.F.);
#8799=ORIENTED_EDGE('',*,*,#6635,.F.);
#8800=ORIENTED_EDGE('',*,*,#6636,.F.);
#8801=ORIENTED_EDGE('',*,*,#6635,.T.);
#8802=ORIENTED_EDGE('',*,*,#6518,.F.);
#8803=ORIENTED_EDGE('',*,*,#6594,.F.);
#8804=ORIENTED_EDGE('',*,*,#6636,.T.);
#8805=ORIENTED_EDGE('',*,*,#6593,.T.);
#8806=ORIENTED_EDGE('',*,*,#6597,.T.);
#8807=ORIENTED_EDGE('',*,*,#6600,.T.);
#8808=ORIENTED_EDGE('',*,*,#6603,.T.);
#8809=ORIENTED_EDGE('',*,*,#6606,.T.);
#8810=ORIENTED_EDGE('',*,*,#6609,.T.);
#8811=ORIENTED_EDGE('',*,*,#6612,.T.);
#8812=ORIENTED_EDGE('',*,*,#6615,.T.);
#8813=ORIENTED_EDGE('',*,*,#6618,.T.);
#8814=ORIENTED_EDGE('',*,*,#6620,.T.);
#8815=ORIENTED_EDGE('',*,*,#6622,.T.);
#8816=ORIENTED_EDGE('',*,*,#6624,.T.);
#8817=ORIENTED_EDGE('',*,*,#6626,.T.);
#8818=ORIENTED_EDGE('',*,*,#6628,.T.);
#8819=ORIENTED_EDGE('',*,*,#6630,.T.);
#8820=ORIENTED_EDGE('',*,*,#6632,.T.);
#8821=ORIENTED_EDGE('',*,*,#6634,.T.);
#8822=ORIENTED_EDGE('',*,*,#6595,.T.);
#8823=ORIENTED_EDGE('',*,*,#6637,.T.);
#8824=ORIENTED_EDGE('',*,*,#6598,.T.);
#8825=ORIENTED_EDGE('',*,*,#6638,.T.);
#8826=ORIENTED_EDGE('',*,*,#6601,.T.);
#8827=ORIENTED_EDGE('',*,*,#6639,.T.);
#8828=ORIENTED_EDGE('',*,*,#6604,.T.);
#8829=ORIENTED_EDGE('',*,*,#6640,.T.);
#8830=ORIENTED_EDGE('',*,*,#6607,.T.);
#8831=ORIENTED_EDGE('',*,*,#6641,.T.);
#8832=ORIENTED_EDGE('',*,*,#6610,.T.);
#8833=ORIENTED_EDGE('',*,*,#6642,.T.);
#8834=ORIENTED_EDGE('',*,*,#6613,.T.);
#8835=ORIENTED_EDGE('',*,*,#6643,.T.);
#8836=ORIENTED_EDGE('',*,*,#6616,.T.);
#8837=ORIENTED_EDGE('',*,*,#6644,.T.);
#8838=ORIENTED_EDGE('',*,*,#6645,.F.);
#8839=ORIENTED_EDGE('',*,*,#6646,.T.);
#8840=ORIENTED_EDGE('',*,*,#6539,.F.);
#8841=ORIENTED_EDGE('',*,*,#6592,.F.);
#8842=ORIENTED_EDGE('',*,*,#6591,.F.);
#8843=ORIENTED_EDGE('',*,*,#6590,.F.);
#8844=ORIENTED_EDGE('',*,*,#6589,.F.);
#8845=ORIENTED_EDGE('',*,*,#6588,.F.);
#8846=ORIENTED_EDGE('',*,*,#6587,.F.);
#8847=ORIENTED_EDGE('',*,*,#6586,.F.);
#8848=ORIENTED_EDGE('',*,*,#6585,.F.);
#8849=ORIENTED_EDGE('',*,*,#6528,.F.);
#8850=ORIENTED_EDGE('',*,*,#6644,.F.);
#8851=ORIENTED_EDGE('',*,*,#6643,.F.);
#8852=ORIENTED_EDGE('',*,*,#6642,.F.);
#8853=ORIENTED_EDGE('',*,*,#6641,.F.);
#8854=ORIENTED_EDGE('',*,*,#6640,.F.);
#8855=ORIENTED_EDGE('',*,*,#6639,.F.);
#8856=ORIENTED_EDGE('',*,*,#6638,.F.);
#8857=ORIENTED_EDGE('',*,*,#6637,.F.);
#8858=ORIENTED_EDGE('',*,*,#6517,.F.);
#8859=ORIENTED_EDGE('',*,*,#6516,.F.);
#8860=ORIENTED_EDGE('',*,*,#6515,.F.);
#8861=ORIENTED_EDGE('',*,*,#6514,.F.);
#8862=ORIENTED_EDGE('',*,*,#6513,.F.);
#8863=ORIENTED_EDGE('',*,*,#6512,.F.);
#8864=ORIENTED_EDGE('',*,*,#6511,.F.);
#8865=ORIENTED_EDGE('',*,*,#6510,.F.);
#8866=ORIENTED_EDGE('',*,*,#6509,.F.);
#8867=ORIENTED_EDGE('',*,*,#6540,.F.);
#8868=ORIENTED_EDGE('',*,*,#6646,.F.);
#8869=ORIENTED_EDGE('',*,*,#6451,.T.);
#8870=ORIENTED_EDGE('',*,*,#6645,.T.);
#8871=ORIENTED_EDGE('',*,*,#6452,.T.);
#8872=ORIENTED_EDGE('',*,*,#6647,.F.);
#8873=ORIENTED_EDGE('',*,*,#6648,.F.);
#8874=ORIENTED_EDGE('',*,*,#6649,.T.);
#8875=ORIENTED_EDGE('',*,*,#6650,.F.);
#8876=ORIENTED_EDGE('',*,*,#6651,.F.);
#8877=ORIENTED_EDGE('',*,*,#6649,.F.);
#8878=ORIENTED_EDGE('',*,*,#6652,.F.);
#8879=ORIENTED_EDGE('',*,*,#6653,.T.);
#8880=ORIENTED_EDGE('',*,*,#6654,.F.);
#8881=ORIENTED_EDGE('',*,*,#6653,.F.);
#8882=ORIENTED_EDGE('',*,*,#6647,.T.);
#8883=ORIENTED_EDGE('',*,*,#6648,.T.);
#8884=ORIENTED_EDGE('',*,*,#6655,.T.);
#8885=ORIENTED_EDGE('',*,*,#6656,.T.);
#8886=ORIENTED_EDGE('',*,*,#6657,.F.);
#8887=ORIENTED_EDGE('',*,*,#6658,.F.);
#8888=ORIENTED_EDGE('',*,*,#6659,.T.);
#8889=ORIENTED_EDGE('',*,*,#6658,.T.);
#8890=ORIENTED_EDGE('',*,*,#6660,.F.);
#8891=ORIENTED_EDGE('',*,*,#6661,.F.);
#8892=ORIENTED_EDGE('',*,*,#6662,.T.);
#8893=ORIENTED_EDGE('',*,*,#6661,.T.);
#8894=ORIENTED_EDGE('',*,*,#6663,.F.);
#8895=ORIENTED_EDGE('',*,*,#6664,.F.);
#8896=ORIENTED_EDGE('',*,*,#6665,.T.);
#8897=ORIENTED_EDGE('',*,*,#6664,.T.);
#8898=ORIENTED_EDGE('',*,*,#6666,.F.);
#8899=ORIENTED_EDGE('',*,*,#6667,.F.);
#8900=ORIENTED_EDGE('',*,*,#6668,.T.);
#8901=ORIENTED_EDGE('',*,*,#6667,.T.);
#8902=ORIENTED_EDGE('',*,*,#6669,.F.);
#8903=ORIENTED_EDGE('',*,*,#6670,.F.);
#8904=ORIENTED_EDGE('',*,*,#6671,.T.);
#8905=ORIENTED_EDGE('',*,*,#6670,.T.);
#8906=ORIENTED_EDGE('',*,*,#6672,.F.);
#8907=ORIENTED_EDGE('',*,*,#6673,.F.);
#8908=ORIENTED_EDGE('',*,*,#6674,.T.);
#8909=ORIENTED_EDGE('',*,*,#6673,.T.);
#8910=ORIENTED_EDGE('',*,*,#6675,.F.);
#8911=ORIENTED_EDGE('',*,*,#6676,.F.);
#8912=ORIENTED_EDGE('',*,*,#6677,.T.);
#8913=ORIENTED_EDGE('',*,*,#6676,.T.);
#8914=ORIENTED_EDGE('',*,*,#6678,.F.);
#8915=ORIENTED_EDGE('',*,*,#6679,.F.);
#8916=ORIENTED_EDGE('',*,*,#6680,.T.);
#8917=ORIENTED_EDGE('',*,*,#6679,.T.);
#8918=ORIENTED_EDGE('',*,*,#6681,.F.);
#8919=ORIENTED_EDGE('',*,*,#6682,.F.);
#8920=ORIENTED_EDGE('',*,*,#6683,.T.);
#8921=ORIENTED_EDGE('',*,*,#6682,.T.);
#8922=ORIENTED_EDGE('',*,*,#6684,.F.);
#8923=ORIENTED_EDGE('',*,*,#6685,.F.);
#8924=ORIENTED_EDGE('',*,*,#6686,.T.);
#8925=ORIENTED_EDGE('',*,*,#6685,.T.);
#8926=ORIENTED_EDGE('',*,*,#6687,.F.);
#8927=ORIENTED_EDGE('',*,*,#6688,.F.);
#8928=ORIENTED_EDGE('',*,*,#6689,.T.);
#8929=ORIENTED_EDGE('',*,*,#6688,.T.);
#8930=ORIENTED_EDGE('',*,*,#6690,.F.);
#8931=ORIENTED_EDGE('',*,*,#6691,.F.);
#8932=ORIENTED_EDGE('',*,*,#6692,.T.);
#8933=ORIENTED_EDGE('',*,*,#6691,.T.);
#8934=ORIENTED_EDGE('',*,*,#6693,.F.);
#8935=ORIENTED_EDGE('',*,*,#6694,.F.);
#8936=ORIENTED_EDGE('',*,*,#6695,.T.);
#8937=ORIENTED_EDGE('',*,*,#6694,.T.);
#8938=ORIENTED_EDGE('',*,*,#6696,.F.);
#8939=ORIENTED_EDGE('',*,*,#6697,.F.);
#8940=ORIENTED_EDGE('',*,*,#6698,.T.);
#8941=ORIENTED_EDGE('',*,*,#6697,.T.);
#8942=ORIENTED_EDGE('',*,*,#6699,.F.);
#8943=ORIENTED_EDGE('',*,*,#6700,.F.);
#8944=ORIENTED_EDGE('',*,*,#6701,.T.);
#8945=ORIENTED_EDGE('',*,*,#6700,.T.);
#8946=ORIENTED_EDGE('',*,*,#6702,.F.);
#8947=ORIENTED_EDGE('',*,*,#6703,.F.);
#8948=ORIENTED_EDGE('',*,*,#6704,.T.);
#8949=ORIENTED_EDGE('',*,*,#6703,.T.);
#8950=ORIENTED_EDGE('',*,*,#6705,.F.);
#8951=ORIENTED_EDGE('',*,*,#6706,.F.);
#8952=ORIENTED_EDGE('',*,*,#6707,.T.);
#8953=ORIENTED_EDGE('',*,*,#6706,.T.);
#8954=ORIENTED_EDGE('',*,*,#6708,.F.);
#8955=ORIENTED_EDGE('',*,*,#6656,.F.);
#8956=ORIENTED_EDGE('',*,*,#6707,.F.);
#8957=ORIENTED_EDGE('',*,*,#6655,.F.);
#8958=ORIENTED_EDGE('',*,*,#6659,.F.);
#8959=ORIENTED_EDGE('',*,*,#6662,.F.);
#8960=ORIENTED_EDGE('',*,*,#6665,.F.);
#8961=ORIENTED_EDGE('',*,*,#6668,.F.);
#8962=ORIENTED_EDGE('',*,*,#6671,.F.);
#8963=ORIENTED_EDGE('',*,*,#6674,.F.);
#8964=ORIENTED_EDGE('',*,*,#6677,.F.);
#8965=ORIENTED_EDGE('',*,*,#6680,.F.);
#8966=ORIENTED_EDGE('',*,*,#6683,.F.);
#8967=ORIENTED_EDGE('',*,*,#6686,.F.);
#8968=ORIENTED_EDGE('',*,*,#6689,.F.);
#8969=ORIENTED_EDGE('',*,*,#6692,.F.);
#8970=ORIENTED_EDGE('',*,*,#6695,.F.);
#8971=ORIENTED_EDGE('',*,*,#6698,.F.);
#8972=ORIENTED_EDGE('',*,*,#6701,.F.);
#8973=ORIENTED_EDGE('',*,*,#6704,.F.);
#8974=ORIENTED_EDGE('',*,*,#6705,.T.);
#8975=ORIENTED_EDGE('',*,*,#6709,.F.);
#8976=ORIENTED_EDGE('',*,*,#6702,.T.);
#8977=ORIENTED_EDGE('',*,*,#6710,.F.);
#8978=ORIENTED_EDGE('',*,*,#6699,.T.);
#8979=ORIENTED_EDGE('',*,*,#6711,.F.);
#8980=ORIENTED_EDGE('',*,*,#6696,.T.);
#8981=ORIENTED_EDGE('',*,*,#6712,.F.);
#8982=ORIENTED_EDGE('',*,*,#6693,.T.);
#8983=ORIENTED_EDGE('',*,*,#6713,.F.);
#8984=ORIENTED_EDGE('',*,*,#6690,.T.);
#8985=ORIENTED_EDGE('',*,*,#6714,.F.);
#8986=ORIENTED_EDGE('',*,*,#6681,.T.);
#8987=ORIENTED_EDGE('',*,*,#6678,.T.);
#8988=ORIENTED_EDGE('',*,*,#6675,.T.);
#8989=ORIENTED_EDGE('',*,*,#6672,.T.);
#8990=ORIENTED_EDGE('',*,*,#6669,.T.);
#8991=ORIENTED_EDGE('',*,*,#6666,.T.);
#8992=ORIENTED_EDGE('',*,*,#6663,.T.);
#8993=ORIENTED_EDGE('',*,*,#6660,.T.);
#8994=ORIENTED_EDGE('',*,*,#6657,.T.);
#8995=ORIENTED_EDGE('',*,*,#6708,.T.);
#8996=ORIENTED_EDGE('',*,*,#6715,.F.);
#8997=ORIENTED_EDGE('',*,*,#6716,.F.);
#8998=ORIENTED_EDGE('',*,*,#6717,.T.);
#8999=ORIENTED_EDGE('',*,*,#6718,.T.);
#9000=ORIENTED_EDGE('',*,*,#6719,.T.);
#9001=ORIENTED_EDGE('',*,*,#6720,.T.);
#9002=ORIENTED_EDGE('',*,*,#6721,.T.);
#9003=ORIENTED_EDGE('',*,*,#6722,.T.);
#9004=ORIENTED_EDGE('',*,*,#6723,.T.);
#9005=ORIENTED_EDGE('',*,*,#6724,.T.);
#9006=ORIENTED_EDGE('',*,*,#6725,.T.);
#9007=ORIENTED_EDGE('',*,*,#6726,.T.);
#9008=ORIENTED_EDGE('',*,*,#6727,.F.);
#9009=ORIENTED_EDGE('',*,*,#6728,.T.);
#9010=ORIENTED_EDGE('',*,*,#6729,.T.);
#9011=ORIENTED_EDGE('',*,*,#6730,.T.);
#9012=ORIENTED_EDGE('',*,*,#6731,.T.);
#9013=ORIENTED_EDGE('',*,*,#6732,.T.);
#9014=ORIENTED_EDGE('',*,*,#6733,.T.);
#9015=ORIENTED_EDGE('',*,*,#6734,.T.);
#9016=ORIENTED_EDGE('',*,*,#6735,.T.);
#9017=ORIENTED_EDGE('',*,*,#6736,.T.);
#9018=ORIENTED_EDGE('',*,*,#6737,.T.);
#9019=ORIENTED_EDGE('',*,*,#6738,.F.);
#9020=ORIENTED_EDGE('',*,*,#6652,.T.);
#9021=ORIENTED_EDGE('',*,*,#6684,.T.);
#9022=ORIENTED_EDGE('',*,*,#6739,.F.);
#9023=ORIENTED_EDGE('',*,*,#6687,.T.);
#9024=ORIENTED_EDGE('',*,*,#6740,.F.);
#9025=ORIENTED_EDGE('',*,*,#6741,.T.);
#9026=ORIENTED_EDGE('',*,*,#6742,.T.);
#9027=ORIENTED_EDGE('',*,*,#6725,.F.);
#9028=ORIENTED_EDGE('',*,*,#6743,.F.);
#9029=ORIENTED_EDGE('',*,*,#6744,.T.);
#9030=ORIENTED_EDGE('',*,*,#6743,.T.);
#9031=ORIENTED_EDGE('',*,*,#6724,.F.);
#9032=ORIENTED_EDGE('',*,*,#6745,.F.);
#9033=ORIENTED_EDGE('',*,*,#6746,.T.);
#9034=ORIENTED_EDGE('',*,*,#6745,.T.);
#9035=ORIENTED_EDGE('',*,*,#6723,.F.);
#9036=ORIENTED_EDGE('',*,*,#6747,.F.);
#9037=ORIENTED_EDGE('',*,*,#6748,.T.);
#9038=ORIENTED_EDGE('',*,*,#6747,.T.);
#9039=ORIENTED_EDGE('',*,*,#6722,.F.);
#9040=ORIENTED_EDGE('',*,*,#6749,.F.);
#9041=ORIENTED_EDGE('',*,*,#6750,.T.);
#9042=ORIENTED_EDGE('',*,*,#6749,.T.);
#9043=ORIENTED_EDGE('',*,*,#6721,.F.);
#9044=ORIENTED_EDGE('',*,*,#6751,.F.);
#9045=ORIENTED_EDGE('',*,*,#6752,.T.);
#9046=ORIENTED_EDGE('',*,*,#6751,.T.);
#9047=ORIENTED_EDGE('',*,*,#6720,.F.);
#9048=ORIENTED_EDGE('',*,*,#6753,.F.);
#9049=ORIENTED_EDGE('',*,*,#6754,.T.);
#9050=ORIENTED_EDGE('',*,*,#6753,.T.);
#9051=ORIENTED_EDGE('',*,*,#6719,.F.);
#9052=ORIENTED_EDGE('',*,*,#6755,.F.);
#9053=ORIENTED_EDGE('',*,*,#6756,.T.);
#9054=ORIENTED_EDGE('',*,*,#6755,.T.);
#9055=ORIENTED_EDGE('',*,*,#6718,.F.);
#9056=ORIENTED_EDGE('',*,*,#6757,.F.);
#9057=ORIENTED_EDGE('',*,*,#6758,.T.);
#9058=ORIENTED_EDGE('',*,*,#6757,.T.);
#9059=ORIENTED_EDGE('',*,*,#6717,.F.);
#9060=ORIENTED_EDGE('',*,*,#6759,.F.);
#9061=ORIENTED_EDGE('',*,*,#6760,.T.);
#9062=ORIENTED_EDGE('',*,*,#6759,.T.);
#9063=ORIENTED_EDGE('',*,*,#6761,.F.);
#9064=ORIENTED_EDGE('',*,*,#6762,.F.);
#9065=ORIENTED_EDGE('',*,*,#6763,.T.);
#9066=ORIENTED_EDGE('',*,*,#6762,.T.);
#9067=ORIENTED_EDGE('',*,*,#6764,.F.);
#9068=ORIENTED_EDGE('',*,*,#6765,.F.);
#9069=ORIENTED_EDGE('',*,*,#6766,.T.);
#9070=ORIENTED_EDGE('',*,*,#6765,.T.);
#9071=ORIENTED_EDGE('',*,*,#6767,.F.);
#9072=ORIENTED_EDGE('',*,*,#6768,.F.);
#9073=ORIENTED_EDGE('',*,*,#6769,.T.);
#9074=ORIENTED_EDGE('',*,*,#6768,.T.);
#9075=ORIENTED_EDGE('',*,*,#6770,.F.);
#9076=ORIENTED_EDGE('',*,*,#6771,.F.);
#9077=ORIENTED_EDGE('',*,*,#6772,.T.);
#9078=ORIENTED_EDGE('',*,*,#6771,.T.);
#9079=ORIENTED_EDGE('',*,*,#6773,.F.);
#9080=ORIENTED_EDGE('',*,*,#6774,.F.);
#9081=ORIENTED_EDGE('',*,*,#6775,.T.);
#9082=ORIENTED_EDGE('',*,*,#6774,.T.);
#9083=ORIENTED_EDGE('',*,*,#6776,.F.);
#9084=ORIENTED_EDGE('',*,*,#6777,.F.);
#9085=ORIENTED_EDGE('',*,*,#6778,.T.);
#9086=ORIENTED_EDGE('',*,*,#6777,.T.);
#9087=ORIENTED_EDGE('',*,*,#6779,.F.);
#9088=ORIENTED_EDGE('',*,*,#6780,.F.);
#9089=ORIENTED_EDGE('',*,*,#6781,.T.);
#9090=ORIENTED_EDGE('',*,*,#6780,.T.);
#9091=ORIENTED_EDGE('',*,*,#6782,.F.);
#9092=ORIENTED_EDGE('',*,*,#6783,.F.);
#9093=ORIENTED_EDGE('',*,*,#6784,.T.);
#9094=ORIENTED_EDGE('',*,*,#6783,.T.);
#9095=ORIENTED_EDGE('',*,*,#6726,.F.);
#9096=ORIENTED_EDGE('',*,*,#6742,.F.);
#9097=ORIENTED_EDGE('',*,*,#6784,.F.);
#9098=ORIENTED_EDGE('',*,*,#6741,.F.);
#9099=ORIENTED_EDGE('',*,*,#6744,.F.);
#9100=ORIENTED_EDGE('',*,*,#6746,.F.);
#9101=ORIENTED_EDGE('',*,*,#6748,.F.);
#9102=ORIENTED_EDGE('',*,*,#6750,.F.);
#9103=ORIENTED_EDGE('',*,*,#6752,.F.);
#9104=ORIENTED_EDGE('',*,*,#6754,.F.);
#9105=ORIENTED_EDGE('',*,*,#6756,.F.);
#9106=ORIENTED_EDGE('',*,*,#6758,.F.);
#9107=ORIENTED_EDGE('',*,*,#6760,.F.);
#9108=ORIENTED_EDGE('',*,*,#6763,.F.);
#9109=ORIENTED_EDGE('',*,*,#6766,.F.);
#9110=ORIENTED_EDGE('',*,*,#6769,.F.);
#9111=ORIENTED_EDGE('',*,*,#6772,.F.);
#9112=ORIENTED_EDGE('',*,*,#6775,.F.);
#9113=ORIENTED_EDGE('',*,*,#6778,.F.);
#9114=ORIENTED_EDGE('',*,*,#6781,.F.);
#9115=ORIENTED_EDGE('',*,*,#6782,.T.);
#9116=ORIENTED_EDGE('',*,*,#6785,.F.);
#9117=ORIENTED_EDGE('',*,*,#6779,.T.);
#9118=ORIENTED_EDGE('',*,*,#6786,.F.);
#9119=ORIENTED_EDGE('',*,*,#6776,.T.);
#9120=ORIENTED_EDGE('',*,*,#6787,.F.);
#9121=ORIENTED_EDGE('',*,*,#6773,.T.);
#9122=ORIENTED_EDGE('',*,*,#6788,.F.);
#9123=ORIENTED_EDGE('',*,*,#6770,.T.);
#9124=ORIENTED_EDGE('',*,*,#6789,.F.);
#9125=ORIENTED_EDGE('',*,*,#6767,.T.);
#9126=ORIENTED_EDGE('',*,*,#6790,.F.);
#9127=ORIENTED_EDGE('',*,*,#6761,.T.);
#9128=ORIENTED_EDGE('',*,*,#6791,.F.);
#9129=ORIENTED_EDGE('',*,*,#6764,.T.);
#9130=ORIENTED_EDGE('',*,*,#6792,.F.);
#9131=ORIENTED_EDGE('',*,*,#6793,.T.);
#9132=ORIENTED_EDGE('',*,*,#6794,.T.);
#9133=ORIENTED_EDGE('',*,*,#6736,.F.);
#9134=ORIENTED_EDGE('',*,*,#6795,.F.);
#9135=ORIENTED_EDGE('',*,*,#6796,.T.);
#9136=ORIENTED_EDGE('',*,*,#6795,.T.);
#9137=ORIENTED_EDGE('',*,*,#6735,.F.);
#9138=ORIENTED_EDGE('',*,*,#6797,.F.);
#9139=ORIENTED_EDGE('',*,*,#6798,.T.);
#9140=ORIENTED_EDGE('',*,*,#6797,.T.);
#9141=ORIENTED_EDGE('',*,*,#6734,.F.);
#9142=ORIENTED_EDGE('',*,*,#6799,.F.);
#9143=ORIENTED_EDGE('',*,*,#6800,.T.);
#9144=ORIENTED_EDGE('',*,*,#6799,.T.);
#9145=ORIENTED_EDGE('',*,*,#6733,.F.);
#9146=ORIENTED_EDGE('',*,*,#6801,.F.);
#9147=ORIENTED_EDGE('',*,*,#6802,.T.);
#9148=ORIENTED_EDGE('',*,*,#6801,.T.);
#9149=ORIENTED_EDGE('',*,*,#6732,.F.);
#9150=ORIENTED_EDGE('',*,*,#6803,.F.);
#9151=ORIENTED_EDGE('',*,*,#6804,.T.);
#9152=ORIENTED_EDGE('',*,*,#6803,.T.);
#9153=ORIENTED_EDGE('',*,*,#6731,.F.);
#9154=ORIENTED_EDGE('',*,*,#6805,.F.);
#9155=ORIENTED_EDGE('',*,*,#6806,.T.);
#9156=ORIENTED_EDGE('',*,*,#6805,.T.);
#9157=ORIENTED_EDGE('',*,*,#6730,.F.);
#9158=ORIENTED_EDGE('',*,*,#6807,.F.);
#9159=ORIENTED_EDGE('',*,*,#6808,.T.);
#9160=ORIENTED_EDGE('',*,*,#6807,.T.);
#9161=ORIENTED_EDGE('',*,*,#6729,.F.);
#9162=ORIENTED_EDGE('',*,*,#6809,.F.);
#9163=ORIENTED_EDGE('',*,*,#6810,.T.);
#9164=ORIENTED_EDGE('',*,*,#6809,.T.);
#9165=ORIENTED_EDGE('',*,*,#6728,.F.);
#9166=ORIENTED_EDGE('',*,*,#6811,.F.);
#9167=ORIENTED_EDGE('',*,*,#6812,.T.);
#9168=ORIENTED_EDGE('',*,*,#6811,.T.);
#9169=ORIENTED_EDGE('',*,*,#6813,.F.);
#9170=ORIENTED_EDGE('',*,*,#6814,.F.);
#9171=ORIENTED_EDGE('',*,*,#6815,.T.);
#9172=ORIENTED_EDGE('',*,*,#6814,.T.);
#9173=ORIENTED_EDGE('',*,*,#6816,.F.);
#9174=ORIENTED_EDGE('',*,*,#6817,.F.);
#9175=ORIENTED_EDGE('',*,*,#6818,.T.);
#9176=ORIENTED_EDGE('',*,*,#6817,.T.);
#9177=ORIENTED_EDGE('',*,*,#6819,.F.);
#9178=ORIENTED_EDGE('',*,*,#6820,.F.);
#9179=ORIENTED_EDGE('',*,*,#6821,.T.);
#9180=ORIENTED_EDGE('',*,*,#6820,.T.);
#9181=ORIENTED_EDGE('',*,*,#6822,.F.);
#9182=ORIENTED_EDGE('',*,*,#6823,.F.);
#9183=ORIENTED_EDGE('',*,*,#6824,.T.);
#9184=ORIENTED_EDGE('',*,*,#6823,.T.);
#9185=ORIENTED_EDGE('',*,*,#6825,.F.);
#9186=ORIENTED_EDGE('',*,*,#6826,.F.);
#9187=ORIENTED_EDGE('',*,*,#6827,.T.);
#9188=ORIENTED_EDGE('',*,*,#6826,.T.);
#9189=ORIENTED_EDGE('',*,*,#6828,.F.);
#9190=ORIENTED_EDGE('',*,*,#6829,.F.);
#9191=ORIENTED_EDGE('',*,*,#6830,.T.);
#9192=ORIENTED_EDGE('',*,*,#6829,.T.);
#9193=ORIENTED_EDGE('',*,*,#6831,.F.);
#9194=ORIENTED_EDGE('',*,*,#6832,.F.);
#9195=ORIENTED_EDGE('',*,*,#6833,.T.);
#9196=ORIENTED_EDGE('',*,*,#6832,.T.);
#9197=ORIENTED_EDGE('',*,*,#6834,.F.);
#9198=ORIENTED_EDGE('',*,*,#6835,.F.);
#9199=ORIENTED_EDGE('',*,*,#6836,.T.);
#9200=ORIENTED_EDGE('',*,*,#6835,.T.);
#9201=ORIENTED_EDGE('',*,*,#6737,.F.);
#9202=ORIENTED_EDGE('',*,*,#6794,.F.);
#9203=ORIENTED_EDGE('',*,*,#6836,.F.);
#9204=ORIENTED_EDGE('',*,*,#6793,.F.);
#9205=ORIENTED_EDGE('',*,*,#6796,.F.);
#9206=ORIENTED_EDGE('',*,*,#6798,.F.);
#9207=ORIENTED_EDGE('',*,*,#6800,.F.);
#9208=ORIENTED_EDGE('',*,*,#6802,.F.);
#9209=ORIENTED_EDGE('',*,*,#6804,.F.);
#9210=ORIENTED_EDGE('',*,*,#6806,.F.);
#9211=ORIENTED_EDGE('',*,*,#6808,.F.);
#9212=ORIENTED_EDGE('',*,*,#6810,.F.);
#9213=ORIENTED_EDGE('',*,*,#6812,.F.);
#9214=ORIENTED_EDGE('',*,*,#6815,.F.);
#9215=ORIENTED_EDGE('',*,*,#6818,.F.);
#9216=ORIENTED_EDGE('',*,*,#6821,.F.);
#9217=ORIENTED_EDGE('',*,*,#6824,.F.);
#9218=ORIENTED_EDGE('',*,*,#6827,.F.);
#9219=ORIENTED_EDGE('',*,*,#6830,.F.);
#9220=ORIENTED_EDGE('',*,*,#6833,.F.);
#9221=ORIENTED_EDGE('',*,*,#6834,.T.);
#9222=ORIENTED_EDGE('',*,*,#6837,.F.);
#9223=ORIENTED_EDGE('',*,*,#6831,.T.);
#9224=ORIENTED_EDGE('',*,*,#6838,.F.);
#9225=ORIENTED_EDGE('',*,*,#6828,.T.);
#9226=ORIENTED_EDGE('',*,*,#6839,.F.);
#9227=ORIENTED_EDGE('',*,*,#6825,.T.);
#9228=ORIENTED_EDGE('',*,*,#6840,.F.);
#9229=ORIENTED_EDGE('',*,*,#6822,.T.);
#9230=ORIENTED_EDGE('',*,*,#6841,.F.);
#9231=ORIENTED_EDGE('',*,*,#6819,.T.);
#9232=ORIENTED_EDGE('',*,*,#6842,.F.);
#9233=ORIENTED_EDGE('',*,*,#6813,.T.);
#9234=ORIENTED_EDGE('',*,*,#6843,.F.);
#9235=ORIENTED_EDGE('',*,*,#6816,.T.);
#9236=ORIENTED_EDGE('',*,*,#6844,.F.);
#9237=ORIENTED_EDGE('',*,*,#6845,.F.);
#9238=ORIENTED_EDGE('',*,*,#6846,.T.);
#9239=ORIENTED_EDGE('',*,*,#6715,.T.);
#9240=ORIENTED_EDGE('',*,*,#6709,.T.);
#9241=ORIENTED_EDGE('',*,*,#6710,.T.);
#9242=ORIENTED_EDGE('',*,*,#6711,.T.);
#9243=ORIENTED_EDGE('',*,*,#6712,.T.);
#9244=ORIENTED_EDGE('',*,*,#6713,.T.);
#9245=ORIENTED_EDGE('',*,*,#6714,.T.);
#9246=ORIENTED_EDGE('',*,*,#6740,.T.);
#9247=ORIENTED_EDGE('',*,*,#6739,.T.);
#9248=ORIENTED_EDGE('',*,*,#6738,.T.);
#9249=ORIENTED_EDGE('',*,*,#6837,.T.);
#9250=ORIENTED_EDGE('',*,*,#6838,.T.);
#9251=ORIENTED_EDGE('',*,*,#6839,.T.);
#9252=ORIENTED_EDGE('',*,*,#6840,.T.);
#9253=ORIENTED_EDGE('',*,*,#6841,.T.);
#9254=ORIENTED_EDGE('',*,*,#6842,.T.);
#9255=ORIENTED_EDGE('',*,*,#6844,.T.);
#9256=ORIENTED_EDGE('',*,*,#6843,.T.);
#9257=ORIENTED_EDGE('',*,*,#6727,.T.);
#9258=ORIENTED_EDGE('',*,*,#6785,.T.);
#9259=ORIENTED_EDGE('',*,*,#6786,.T.);
#9260=ORIENTED_EDGE('',*,*,#6787,.T.);
#9261=ORIENTED_EDGE('',*,*,#6788,.T.);
#9262=ORIENTED_EDGE('',*,*,#6789,.T.);
#9263=ORIENTED_EDGE('',*,*,#6790,.T.);
#9264=ORIENTED_EDGE('',*,*,#6792,.T.);
#9265=ORIENTED_EDGE('',*,*,#6791,.T.);
#9266=ORIENTED_EDGE('',*,*,#6716,.T.);
#9267=ORIENTED_EDGE('',*,*,#6846,.F.);
#9268=ORIENTED_EDGE('',*,*,#6650,.T.);
#9269=ORIENTED_EDGE('',*,*,#6651,.T.);
#9270=ORIENTED_EDGE('',*,*,#6845,.T.);
#9271=ORIENTED_EDGE('',*,*,#6654,.T.);
#9272=ORIENTED_EDGE('',*,*,#6847,.F.);
#9273=ORIENTED_EDGE('',*,*,#6848,.F.);
#9274=ORIENTED_EDGE('',*,*,#6849,.F.);
#9275=ORIENTED_EDGE('',*,*,#6850,.F.);
#9276=ORIENTED_EDGE('',*,*,#6851,.F.);
#9277=ORIENTED_EDGE('',*,*,#6852,.F.);
#9278=ORIENTED_EDGE('',*,*,#6853,.F.);
#9279=ORIENTED_EDGE('',*,*,#6854,.F.);
#9280=ORIENTED_EDGE('',*,*,#6855,.T.);
#9281=ORIENTED_EDGE('',*,*,#6856,.F.);
#9282=ORIENTED_EDGE('',*,*,#6857,.F.);
#9283=ORIENTED_EDGE('',*,*,#6858,.F.);
#9284=ORIENTED_EDGE('',*,*,#6859,.F.);
#9285=ORIENTED_EDGE('',*,*,#6860,.F.);
#9286=ORIENTED_EDGE('',*,*,#6861,.F.);
#9287=ORIENTED_EDGE('',*,*,#6862,.F.);
#9288=ORIENTED_EDGE('',*,*,#6863,.F.);
#9289=ORIENTED_EDGE('',*,*,#6864,.T.);
#9290=ORIENTED_EDGE('',*,*,#6865,.F.);
#9291=ORIENTED_EDGE('',*,*,#6866,.F.);
#9292=ORIENTED_EDGE('',*,*,#6867,.F.);
#9293=ORIENTED_EDGE('',*,*,#6868,.F.);
#9294=ORIENTED_EDGE('',*,*,#6869,.F.);
#9295=ORIENTED_EDGE('',*,*,#6870,.F.);
#9296=ORIENTED_EDGE('',*,*,#6871,.F.);
#9297=ORIENTED_EDGE('',*,*,#6872,.F.);
#9298=ORIENTED_EDGE('',*,*,#6873,.T.);
#9299=ORIENTED_EDGE('',*,*,#6874,.F.);
#9300=ORIENTED_EDGE('',*,*,#6875,.F.);
#9301=ORIENTED_EDGE('',*,*,#6876,.F.);
#9302=ORIENTED_EDGE('',*,*,#6877,.F.);
#9303=ORIENTED_EDGE('',*,*,#6878,.F.);
#9304=ORIENTED_EDGE('',*,*,#6879,.F.);
#9305=ORIENTED_EDGE('',*,*,#6880,.F.);
#9306=ORIENTED_EDGE('',*,*,#6881,.F.);
#9307=ORIENTED_EDGE('',*,*,#6882,.T.);
#9308=ORIENTED_EDGE('',*,*,#6883,.F.);
#9309=ORIENTED_EDGE('',*,*,#6884,.F.);
#9310=ORIENTED_EDGE('',*,*,#6885,.F.);
#9311=ORIENTED_EDGE('',*,*,#6886,.F.);
#9312=ORIENTED_EDGE('',*,*,#6887,.F.);
#9313=ORIENTED_EDGE('',*,*,#6888,.F.);
#9314=ORIENTED_EDGE('',*,*,#6889,.F.);
#9315=ORIENTED_EDGE('',*,*,#6890,.F.);
#9316=ORIENTED_EDGE('',*,*,#6891,.T.);
#9317=ORIENTED_EDGE('',*,*,#6892,.F.);
#9318=ORIENTED_EDGE('',*,*,#6893,.F.);
#9319=ORIENTED_EDGE('',*,*,#6894,.F.);
#9320=ORIENTED_EDGE('',*,*,#6895,.F.);
#9321=ORIENTED_EDGE('',*,*,#6896,.F.);
#9322=ORIENTED_EDGE('',*,*,#6897,.F.);
#9323=ORIENTED_EDGE('',*,*,#6898,.F.);
#9324=ORIENTED_EDGE('',*,*,#6899,.F.);
#9325=ORIENTED_EDGE('',*,*,#6900,.T.);
#9326=ORIENTED_EDGE('',*,*,#6901,.F.);
#9327=ORIENTED_EDGE('',*,*,#6902,.F.);
#9328=ORIENTED_EDGE('',*,*,#6903,.F.);
#9329=ORIENTED_EDGE('',*,*,#6891,.F.);
#9330=ORIENTED_EDGE('',*,*,#6904,.F.);
#9331=ORIENTED_EDGE('',*,*,#6905,.F.);
#9332=ORIENTED_EDGE('',*,*,#6906,.F.);
#9333=ORIENTED_EDGE('',*,*,#6855,.F.);
#9334=ORIENTED_EDGE('',*,*,#6907,.F.);
#9335=ORIENTED_EDGE('',*,*,#6908,.F.);
#9336=ORIENTED_EDGE('',*,*,#6909,.F.);
#9337=ORIENTED_EDGE('',*,*,#6873,.F.);
#9338=ORIENTED_EDGE('',*,*,#6910,.F.);
#9339=ORIENTED_EDGE('',*,*,#6882,.F.);
#9340=ORIENTED_EDGE('',*,*,#6911,.F.);
#9341=ORIENTED_EDGE('',*,*,#6912,.F.);
#9342=ORIENTED_EDGE('',*,*,#6913,.F.);
#9343=ORIENTED_EDGE('',*,*,#6864,.F.);
#9344=ORIENTED_EDGE('',*,*,#6914,.F.);
#9345=ORIENTED_EDGE('',*,*,#6915,.F.);
#9346=ORIENTED_EDGE('',*,*,#6916,.F.);
#9347=ORIENTED_EDGE('',*,*,#6900,.F.);
#9348=ORIENTED_EDGE('',*,*,#6917,.F.);
#9349=ORIENTED_EDGE('',*,*,#6918,.F.);
#9350=ORIENTED_EDGE('',*,*,#6919,.F.);
#9351=ORIENTED_EDGE('',*,*,#6918,.T.);
#9352=ORIENTED_EDGE('',*,*,#6920,.F.);
#9353=ORIENTED_EDGE('',*,*,#6921,.F.);
#9354=ORIENTED_EDGE('',*,*,#6922,.F.);
#9355=ORIENTED_EDGE('',*,*,#6923,.F.);
#9356=ORIENTED_EDGE('',*,*,#6924,.F.);
#9357=ORIENTED_EDGE('',*,*,#6925,.F.);
#9358=ORIENTED_EDGE('',*,*,#6926,.F.);
#9359=ORIENTED_EDGE('',*,*,#6927,.F.);
#9360=ORIENTED_EDGE('',*,*,#6902,.T.);
#9361=ORIENTED_EDGE('',*,*,#6928,.F.);
#9362=ORIENTED_EDGE('',*,*,#6929,.F.);
#9363=ORIENTED_EDGE('',*,*,#6930,.F.);
#9364=ORIENTED_EDGE('',*,*,#6931,.F.);
#9365=ORIENTED_EDGE('',*,*,#6932,.F.);
#9366=ORIENTED_EDGE('',*,*,#6933,.F.);
#9367=ORIENTED_EDGE('',*,*,#6934,.F.);
#9368=ORIENTED_EDGE('',*,*,#6935,.F.);
#9369=ORIENTED_EDGE('',*,*,#6912,.T.);
#9370=ORIENTED_EDGE('',*,*,#6936,.F.);
#9371=ORIENTED_EDGE('',*,*,#6937,.F.);
#9372=ORIENTED_EDGE('',*,*,#6938,.F.);
#9373=ORIENTED_EDGE('',*,*,#6939,.F.);
#9374=ORIENTED_EDGE('',*,*,#6940,.F.);
#9375=ORIENTED_EDGE('',*,*,#6941,.F.);
#9376=ORIENTED_EDGE('',*,*,#6942,.F.);
#9377=ORIENTED_EDGE('',*,*,#6943,.F.);
#9378=ORIENTED_EDGE('',*,*,#6908,.T.);
#9379=ORIENTED_EDGE('',*,*,#6944,.F.);
#9380=ORIENTED_EDGE('',*,*,#6945,.F.);
#9381=ORIENTED_EDGE('',*,*,#6946,.F.);
#9382=ORIENTED_EDGE('',*,*,#6947,.F.);
#9383=ORIENTED_EDGE('',*,*,#6948,.F.);
#9384=ORIENTED_EDGE('',*,*,#6949,.F.);
#9385=ORIENTED_EDGE('',*,*,#6950,.F.);
#9386=ORIENTED_EDGE('',*,*,#6951,.F.);
#9387=ORIENTED_EDGE('',*,*,#6915,.T.);
#9388=ORIENTED_EDGE('',*,*,#6952,.F.);
#9389=ORIENTED_EDGE('',*,*,#6953,.F.);
#9390=ORIENTED_EDGE('',*,*,#6954,.F.);
#9391=ORIENTED_EDGE('',*,*,#6955,.F.);
#9392=ORIENTED_EDGE('',*,*,#6956,.F.);
#9393=ORIENTED_EDGE('',*,*,#6957,.F.);
#9394=ORIENTED_EDGE('',*,*,#6958,.F.);
#9395=ORIENTED_EDGE('',*,*,#6959,.F.);
#9396=ORIENTED_EDGE('',*,*,#6905,.T.);
#9397=ORIENTED_EDGE('',*,*,#6960,.F.);
#9398=ORIENTED_EDGE('',*,*,#6961,.F.);
#9399=ORIENTED_EDGE('',*,*,#6962,.F.);
#9400=ORIENTED_EDGE('',*,*,#6963,.F.);
#9401=ORIENTED_EDGE('',*,*,#6964,.F.);
#9402=ORIENTED_EDGE('',*,*,#6965,.F.);
#9403=ORIENTED_EDGE('',*,*,#6966,.F.);
#9404=ORIENTED_EDGE('',*,*,#6892,.T.);
#9405=ORIENTED_EDGE('',*,*,#6903,.T.);
#9406=ORIENTED_EDGE('',*,*,#6927,.T.);
#9407=ORIENTED_EDGE('',*,*,#6967,.T.);
#9408=ORIENTED_EDGE('',*,*,#6968,.F.);
#9409=ORIENTED_EDGE('',*,*,#6969,.F.);
#9410=ORIENTED_EDGE('',*,*,#6970,.F.);
#9411=ORIENTED_EDGE('',*,*,#6971,.T.);
#9412=ORIENTED_EDGE('',*,*,#6926,.T.);
#9413=ORIENTED_EDGE('',*,*,#6972,.T.);
#9414=ORIENTED_EDGE('',*,*,#6973,.F.);
#9415=ORIENTED_EDGE('',*,*,#6967,.F.);
#9416=ORIENTED_EDGE('',*,*,#6893,.T.);
#9417=ORIENTED_EDGE('',*,*,#6971,.F.);
#9418=ORIENTED_EDGE('',*,*,#6974,.F.);
#9419=ORIENTED_EDGE('',*,*,#6975,.T.);
#9420=ORIENTED_EDGE('',*,*,#6925,.T.);
#9421=ORIENTED_EDGE('',*,*,#6976,.T.);
#9422=ORIENTED_EDGE('',*,*,#6977,.F.);
#9423=ORIENTED_EDGE('',*,*,#6972,.F.);
#9424=ORIENTED_EDGE('',*,*,#6924,.T.);
#9425=ORIENTED_EDGE('',*,*,#6978,.T.);
#9426=ORIENTED_EDGE('',*,*,#6979,.F.);
#9427=ORIENTED_EDGE('',*,*,#6976,.F.);
#9428=ORIENTED_EDGE('',*,*,#6923,.T.);
#9429=ORIENTED_EDGE('',*,*,#6980,.T.);
#9430=ORIENTED_EDGE('',*,*,#6981,.F.);
#9431=ORIENTED_EDGE('',*,*,#6978,.F.);
#9432=ORIENTED_EDGE('',*,*,#6922,.T.);
#9433=ORIENTED_EDGE('',*,*,#6982,.T.);
#9434=ORIENTED_EDGE('',*,*,#6983,.F.);
#9435=ORIENTED_EDGE('',*,*,#6980,.F.);
#9436=ORIENTED_EDGE('',*,*,#6921,.T.);
#9437=ORIENTED_EDGE('',*,*,#6984,.F.);
#9438=ORIENTED_EDGE('',*,*,#6985,.F.);
#9439=ORIENTED_EDGE('',*,*,#6982,.F.);
#9440=ORIENTED_EDGE('',*,*,#6986,.T.);
#9441=ORIENTED_EDGE('',*,*,#6987,.T.);
#9442=ORIENTED_EDGE('',*,*,#6988,.T.);
#9443=ORIENTED_EDGE('',*,*,#6989,.T.);
#9444=ORIENTED_EDGE('',*,*,#6990,.T.);
#9445=ORIENTED_EDGE('',*,*,#6991,.T.);
#9446=ORIENTED_EDGE('',*,*,#6974,.T.);
#9447=ORIENTED_EDGE('',*,*,#6970,.T.);
#9448=ORIENTED_EDGE('',*,*,#6992,.T.);
#9449=ORIENTED_EDGE('',*,*,#6993,.T.);
#9450=ORIENTED_EDGE('',*,*,#6994,.T.);
#9451=ORIENTED_EDGE('',*,*,#6995,.T.);
#9452=ORIENTED_EDGE('',*,*,#6996,.T.);
#9453=ORIENTED_EDGE('',*,*,#6997,.T.);
#9454=ORIENTED_EDGE('',*,*,#6898,.T.);
#9455=ORIENTED_EDGE('',*,*,#6998,.F.);
#9456=ORIENTED_EDGE('',*,*,#6987,.F.);
#9457=ORIENTED_EDGE('',*,*,#6999,.F.);
#9458=ORIENTED_EDGE('',*,*,#6897,.T.);
#9459=ORIENTED_EDGE('',*,*,#7000,.F.);
#9460=ORIENTED_EDGE('',*,*,#6988,.F.);
#9461=ORIENTED_EDGE('',*,*,#6998,.T.);
#9462=ORIENTED_EDGE('',*,*,#6896,.T.);
#9463=ORIENTED_EDGE('',*,*,#7001,.F.);
#9464=ORIENTED_EDGE('',*,*,#6989,.F.);
#9465=ORIENTED_EDGE('',*,*,#7000,.T.);
#9466=ORIENTED_EDGE('',*,*,#6895,.T.);
#9467=ORIENTED_EDGE('',*,*,#7002,.F.);
#9468=ORIENTED_EDGE('',*,*,#6990,.F.);
#9469=ORIENTED_EDGE('',*,*,#7001,.T.);
#9470=ORIENTED_EDGE('',*,*,#6894,.T.);
#9471=ORIENTED_EDGE('',*,*,#6975,.F.);
#9472=ORIENTED_EDGE('',*,*,#6991,.F.);
#9473=ORIENTED_EDGE('',*,*,#7002,.T.);
#9474=ORIENTED_EDGE('',*,*,#6969,.T.);
#9475=ORIENTED_EDGE('',*,*,#7003,.F.);
#9476=ORIENTED_EDGE('',*,*,#7004,.F.);
#9477=ORIENTED_EDGE('',*,*,#6992,.F.);
#9478=ORIENTED_EDGE('',*,*,#7004,.T.);
#9479=ORIENTED_EDGE('',*,*,#7005,.F.);
#9480=ORIENTED_EDGE('',*,*,#7006,.F.);
#9481=ORIENTED_EDGE('',*,*,#6993,.F.);
#9482=ORIENTED_EDGE('',*,*,#7006,.T.);
#9483=ORIENTED_EDGE('',*,*,#7007,.F.);
#9484=ORIENTED_EDGE('',*,*,#7008,.F.);
#9485=ORIENTED_EDGE('',*,*,#6994,.F.);
#9486=ORIENTED_EDGE('',*,*,#7008,.T.);
#9487=ORIENTED_EDGE('',*,*,#7009,.F.);
#9488=ORIENTED_EDGE('',*,*,#7010,.F.);
#9489=ORIENTED_EDGE('',*,*,#6995,.F.);
#9490=ORIENTED_EDGE('',*,*,#7010,.T.);
#9491=ORIENTED_EDGE('',*,*,#7011,.F.);
#9492=ORIENTED_EDGE('',*,*,#7012,.F.);
#9493=ORIENTED_EDGE('',*,*,#6996,.F.);
#9494=ORIENTED_EDGE('',*,*,#7012,.T.);
#9495=ORIENTED_EDGE('',*,*,#7013,.F.);
#9496=ORIENTED_EDGE('',*,*,#7014,.F.);
#9497=ORIENTED_EDGE('',*,*,#6997,.F.);
#9498=ORIENTED_EDGE('',*,*,#6899,.T.);
#9499=ORIENTED_EDGE('',*,*,#6999,.T.);
#9500=ORIENTED_EDGE('',*,*,#6986,.F.);
#9501=ORIENTED_EDGE('',*,*,#7014,.T.);
#9502=ORIENTED_EDGE('',*,*,#7015,.F.);
#9503=ORIENTED_EDGE('',*,*,#6984,.T.);
#9504=ORIENTED_EDGE('',*,*,#6920,.T.);
#9505=ORIENTED_EDGE('',*,*,#6917,.T.);
#9506=ORIENTED_EDGE('',*,*,#7015,.T.);
#9507=ORIENTED_EDGE('',*,*,#7013,.T.);
#9508=ORIENTED_EDGE('',*,*,#7011,.T.);
#9509=ORIENTED_EDGE('',*,*,#7009,.T.);
#9510=ORIENTED_EDGE('',*,*,#7007,.T.);
#9511=ORIENTED_EDGE('',*,*,#7005,.T.);
#9512=ORIENTED_EDGE('',*,*,#7003,.T.);
#9513=ORIENTED_EDGE('',*,*,#6968,.T.);
#9514=ORIENTED_EDGE('',*,*,#6973,.T.);
#9515=ORIENTED_EDGE('',*,*,#6977,.T.);
#9516=ORIENTED_EDGE('',*,*,#6979,.T.);
#9517=ORIENTED_EDGE('',*,*,#6981,.T.);
#9518=ORIENTED_EDGE('',*,*,#6983,.T.);
#9519=ORIENTED_EDGE('',*,*,#6985,.T.);
#9520=ORIENTED_EDGE('',*,*,#6856,.T.);
#9521=ORIENTED_EDGE('',*,*,#6906,.T.);
#9522=ORIENTED_EDGE('',*,*,#6959,.T.);
#9523=ORIENTED_EDGE('',*,*,#7016,.T.);
#9524=ORIENTED_EDGE('',*,*,#7017,.F.);
#9525=ORIENTED_EDGE('',*,*,#7018,.F.);
#9526=ORIENTED_EDGE('',*,*,#7019,.F.);
#9527=ORIENTED_EDGE('',*,*,#7020,.T.);
#9528=ORIENTED_EDGE('',*,*,#6958,.T.);
#9529=ORIENTED_EDGE('',*,*,#7021,.T.);
#9530=ORIENTED_EDGE('',*,*,#7022,.F.);
#9531=ORIENTED_EDGE('',*,*,#7016,.F.);
#9532=ORIENTED_EDGE('',*,*,#6857,.T.);
#9533=ORIENTED_EDGE('',*,*,#7020,.F.);
#9534=ORIENTED_EDGE('',*,*,#7023,.F.);
#9535=ORIENTED_EDGE('',*,*,#7024,.T.);
#9536=ORIENTED_EDGE('',*,*,#6957,.T.);
#9537=ORIENTED_EDGE('',*,*,#7025,.T.);
#9538=ORIENTED_EDGE('',*,*,#7026,.F.);
#9539=ORIENTED_EDGE('',*,*,#7021,.F.);
#9540=ORIENTED_EDGE('',*,*,#6956,.T.);
#9541=ORIENTED_EDGE('',*,*,#7027,.T.);
#9542=ORIENTED_EDGE('',*,*,#7028,.F.);
#9543=ORIENTED_EDGE('',*,*,#7025,.F.);
#9544=ORIENTED_EDGE('',*,*,#6955,.T.);
#9545=ORIENTED_EDGE('',*,*,#7029,.T.);
#9546=ORIENTED_EDGE('',*,*,#7030,.F.);
#9547=ORIENTED_EDGE('',*,*,#7027,.F.);
#9548=ORIENTED_EDGE('',*,*,#6954,.T.);
#9549=ORIENTED_EDGE('',*,*,#7031,.T.);
#9550=ORIENTED_EDGE('',*,*,#7032,.F.);
#9551=ORIENTED_EDGE('',*,*,#7029,.F.);
#9552=ORIENTED_EDGE('',*,*,#6953,.T.);
#9553=ORIENTED_EDGE('',*,*,#7033,.F.);
#9554=ORIENTED_EDGE('',*,*,#7034,.F.);
#9555=ORIENTED_EDGE('',*,*,#7031,.F.);
#9556=ORIENTED_EDGE('',*,*,#7035,.T.);
#9557=ORIENTED_EDGE('',*,*,#7036,.T.);
#9558=ORIENTED_EDGE('',*,*,#7037,.T.);
#9559=ORIENTED_EDGE('',*,*,#7038,.T.);
#9560=ORIENTED_EDGE('',*,*,#7039,.T.);
#9561=ORIENTED_EDGE('',*,*,#7040,.T.);
#9562=ORIENTED_EDGE('',*,*,#7023,.T.);
#9563=ORIENTED_EDGE('',*,*,#7019,.T.);
#9564=ORIENTED_EDGE('',*,*,#7041,.T.);
#9565=ORIENTED_EDGE('',*,*,#7042,.T.);
#9566=ORIENTED_EDGE('',*,*,#7043,.T.);
#9567=ORIENTED_EDGE('',*,*,#7044,.T.);
#9568=ORIENTED_EDGE('',*,*,#7045,.T.);
#9569=ORIENTED_EDGE('',*,*,#7046,.T.);
#9570=ORIENTED_EDGE('',*,*,#6862,.T.);
#9571=ORIENTED_EDGE('',*,*,#7047,.F.);
#9572=ORIENTED_EDGE('',*,*,#7036,.F.);
#9573=ORIENTED_EDGE('',*,*,#7048,.F.);
#9574=ORIENTED_EDGE('',*,*,#6861,.T.);
#9575=ORIENTED_EDGE('',*,*,#7049,.F.);
#9576=ORIENTED_EDGE('',*,*,#7037,.F.);
#9577=ORIENTED_EDGE('',*,*,#7047,.T.);
#9578=ORIENTED_EDGE('',*,*,#6860,.T.);
#9579=ORIENTED_EDGE('',*,*,#7050,.F.);
#9580=ORIENTED_EDGE('',*,*,#7038,.F.);
#9581=ORIENTED_EDGE('',*,*,#7049,.T.);
#9582=ORIENTED_EDGE('',*,*,#6859,.T.);
#9583=ORIENTED_EDGE('',*,*,#7051,.F.);
#9584=ORIENTED_EDGE('',*,*,#7039,.F.);
#9585=ORIENTED_EDGE('',*,*,#7050,.T.);
#9586=ORIENTED_EDGE('',*,*,#6858,.T.);
#9587=ORIENTED_EDGE('',*,*,#7024,.F.);
#9588=ORIENTED_EDGE('',*,*,#7040,.F.);
#9589=ORIENTED_EDGE('',*,*,#7051,.T.);
#9590=ORIENTED_EDGE('',*,*,#7018,.T.);
#9591=ORIENTED_EDGE('',*,*,#7052,.F.);
#9592=ORIENTED_EDGE('',*,*,#7053,.F.);
#9593=ORIENTED_EDGE('',*,*,#7041,.F.);
#9594=ORIENTED_EDGE('',*,*,#7053,.T.);
#9595=ORIENTED_EDGE('',*,*,#7054,.F.);
#9596=ORIENTED_EDGE('',*,*,#7055,.F.);
#9597=ORIENTED_EDGE('',*,*,#7042,.F.);
#9598=ORIENTED_EDGE('',*,*,#7055,.T.);
#9599=ORIENTED_EDGE('',*,*,#7056,.F.);
#9600=ORIENTED_EDGE('',*,*,#7057,.F.);
#9601=ORIENTED_EDGE('',*,*,#7043,.F.);
#9602=ORIENTED_EDGE('',*,*,#7057,.T.);
#9603=ORIENTED_EDGE('',*,*,#7058,.F.);
#9604=ORIENTED_EDGE('',*,*,#7059,.F.);
#9605=ORIENTED_EDGE('',*,*,#7044,.F.);
#9606=ORIENTED_EDGE('',*,*,#7059,.T.);
#9607=ORIENTED_EDGE('',*,*,#7060,.F.);
#9608=ORIENTED_EDGE('',*,*,#7061,.F.);
#9609=ORIENTED_EDGE('',*,*,#7045,.F.);
#9610=ORIENTED_EDGE('',*,*,#7061,.T.);
#9611=ORIENTED_EDGE('',*,*,#7062,.F.);
#9612=ORIENTED_EDGE('',*,*,#7063,.F.);
#9613=ORIENTED_EDGE('',*,*,#7046,.F.);
#9614=ORIENTED_EDGE('',*,*,#6863,.T.);
#9615=ORIENTED_EDGE('',*,*,#7048,.T.);
#9616=ORIENTED_EDGE('',*,*,#7035,.F.);
#9617=ORIENTED_EDGE('',*,*,#7063,.T.);
#9618=ORIENTED_EDGE('',*,*,#7064,.F.);
#9619=ORIENTED_EDGE('',*,*,#7033,.T.);
#9620=ORIENTED_EDGE('',*,*,#6952,.T.);
#9621=ORIENTED_EDGE('',*,*,#6914,.T.);
#9622=ORIENTED_EDGE('',*,*,#7064,.T.);
#9623=ORIENTED_EDGE('',*,*,#7062,.T.);
#9624=ORIENTED_EDGE('',*,*,#7060,.T.);
#9625=ORIENTED_EDGE('',*,*,#7058,.T.);
#9626=ORIENTED_EDGE('',*,*,#7056,.T.);
#9627=ORIENTED_EDGE('',*,*,#7054,.T.);
#9628=ORIENTED_EDGE('',*,*,#7052,.T.);
#9629=ORIENTED_EDGE('',*,*,#7017,.T.);
#9630=ORIENTED_EDGE('',*,*,#7022,.T.);
#9631=ORIENTED_EDGE('',*,*,#7026,.T.);
#9632=ORIENTED_EDGE('',*,*,#7028,.T.);
#9633=ORIENTED_EDGE('',*,*,#7030,.T.);
#9634=ORIENTED_EDGE('',*,*,#7032,.T.);
#9635=ORIENTED_EDGE('',*,*,#7034,.T.);
#9636=ORIENTED_EDGE('',*,*,#6874,.T.);
#9637=ORIENTED_EDGE('',*,*,#6909,.T.);
#9638=ORIENTED_EDGE('',*,*,#6943,.T.);
#9639=ORIENTED_EDGE('',*,*,#7065,.T.);
#9640=ORIENTED_EDGE('',*,*,#7066,.F.);
#9641=ORIENTED_EDGE('',*,*,#7067,.F.);
#9642=ORIENTED_EDGE('',*,*,#7068,.F.);
#9643=ORIENTED_EDGE('',*,*,#7069,.T.);
#9644=ORIENTED_EDGE('',*,*,#6942,.T.);
#9645=ORIENTED_EDGE('',*,*,#7070,.T.);
#9646=ORIENTED_EDGE('',*,*,#7071,.F.);
#9647=ORIENTED_EDGE('',*,*,#7065,.F.);
#9648=ORIENTED_EDGE('',*,*,#6875,.T.);
#9649=ORIENTED_EDGE('',*,*,#7069,.F.);
#9650=ORIENTED_EDGE('',*,*,#7072,.F.);
#9651=ORIENTED_EDGE('',*,*,#7073,.T.);
#9652=ORIENTED_EDGE('',*,*,#6941,.T.);
#9653=ORIENTED_EDGE('',*,*,#7074,.T.);
#9654=ORIENTED_EDGE('',*,*,#7075,.F.);
#9655=ORIENTED_EDGE('',*,*,#7070,.F.);
#9656=ORIENTED_EDGE('',*,*,#6940,.T.);
#9657=ORIENTED_EDGE('',*,*,#7076,.T.);
#9658=ORIENTED_EDGE('',*,*,#7077,.F.);
#9659=ORIENTED_EDGE('',*,*,#7074,.F.);
#9660=ORIENTED_EDGE('',*,*,#6939,.T.);
#9661=ORIENTED_EDGE('',*,*,#7078,.T.);
#9662=ORIENTED_EDGE('',*,*,#7079,.F.);
#9663=ORIENTED_EDGE('',*,*,#7076,.F.);
#9664=ORIENTED_EDGE('',*,*,#6938,.T.);
#9665=ORIENTED_EDGE('',*,*,#7080,.T.);
#9666=ORIENTED_EDGE('',*,*,#7081,.F.);
#9667=ORIENTED_EDGE('',*,*,#7078,.F.);
#9668=ORIENTED_EDGE('',*,*,#6937,.T.);
#9669=ORIENTED_EDGE('',*,*,#7082,.F.);
#9670=ORIENTED_EDGE('',*,*,#7083,.F.);
#9671=ORIENTED_EDGE('',*,*,#7080,.F.);
#9672=ORIENTED_EDGE('',*,*,#7084,.T.);
#9673=ORIENTED_EDGE('',*,*,#7085,.T.);
#9674=ORIENTED_EDGE('',*,*,#7086,.T.);
#9675=ORIENTED_EDGE('',*,*,#7087,.T.);
#9676=ORIENTED_EDGE('',*,*,#7088,.T.);
#9677=ORIENTED_EDGE('',*,*,#7089,.T.);
#9678=ORIENTED_EDGE('',*,*,#7072,.T.);
#9679=ORIENTED_EDGE('',*,*,#7068,.T.);
#9680=ORIENTED_EDGE('',*,*,#7090,.T.);
#9681=ORIENTED_EDGE('',*,*,#7091,.T.);
#9682=ORIENTED_EDGE('',*,*,#7092,.T.);
#9683=ORIENTED_EDGE('',*,*,#7093,.T.);
#9684=ORIENTED_EDGE('',*,*,#7094,.T.);
#9685=ORIENTED_EDGE('',*,*,#7095,.T.);
#9686=ORIENTED_EDGE('',*,*,#6880,.T.);
#9687=ORIENTED_EDGE('',*,*,#7096,.F.);
#9688=ORIENTED_EDGE('',*,*,#7085,.F.);
#9689=ORIENTED_EDGE('',*,*,#7097,.F.);
#9690=ORIENTED_EDGE('',*,*,#6879,.T.);
#9691=ORIENTED_EDGE('',*,*,#7098,.F.);
#9692=ORIENTED_EDGE('',*,*,#7086,.F.);
#9693=ORIENTED_EDGE('',*,*,#7096,.T.);
#9694=ORIENTED_EDGE('',*,*,#6878,.T.);
#9695=ORIENTED_EDGE('',*,*,#7099,.F.);
#9696=ORIENTED_EDGE('',*,*,#7087,.F.);
#9697=ORIENTED_EDGE('',*,*,#7098,.T.);
#9698=ORIENTED_EDGE('',*,*,#6877,.T.);
#9699=ORIENTED_EDGE('',*,*,#7100,.F.);
#9700=ORIENTED_EDGE('',*,*,#7088,.F.);
#9701=ORIENTED_EDGE('',*,*,#7099,.T.);
#9702=ORIENTED_EDGE('',*,*,#6876,.T.);
#9703=ORIENTED_EDGE('',*,*,#7073,.F.);
#9704=ORIENTED_EDGE('',*,*,#7089,.F.);
#9705=ORIENTED_EDGE('',*,*,#7100,.T.);
#9706=ORIENTED_EDGE('',*,*,#7067,.T.);
#9707=ORIENTED_EDGE('',*,*,#7101,.F.);
#9708=ORIENTED_EDGE('',*,*,#7102,.F.);
#9709=ORIENTED_EDGE('',*,*,#7090,.F.);
#9710=ORIENTED_EDGE('',*,*,#7102,.T.);
#9711=ORIENTED_EDGE('',*,*,#7103,.F.);
#9712=ORIENTED_EDGE('',*,*,#7104,.F.);
#9713=ORIENTED_EDGE('',*,*,#7091,.F.);
#9714=ORIENTED_EDGE('',*,*,#7104,.T.);
#9715=ORIENTED_EDGE('',*,*,#7105,.F.);
#9716=ORIENTED_EDGE('',*,*,#7106,.F.);
#9717=ORIENTED_EDGE('',*,*,#7092,.F.);
#9718=ORIENTED_EDGE('',*,*,#7106,.T.);
#9719=ORIENTED_EDGE('',*,*,#7107,.F.);
#9720=ORIENTED_EDGE('',*,*,#7108,.F.);
#9721=ORIENTED_EDGE('',*,*,#7093,.F.);
#9722=ORIENTED_EDGE('',*,*,#7108,.T.);
#9723=ORIENTED_EDGE('',*,*,#7109,.F.);
#9724=ORIENTED_EDGE('',*,*,#7110,.F.);
#9725=ORIENTED_EDGE('',*,*,#7094,.F.);
#9726=ORIENTED_EDGE('',*,*,#7110,.T.);
#9727=ORIENTED_EDGE('',*,*,#7111,.F.);
#9728=ORIENTED_EDGE('',*,*,#7112,.F.);
#9729=ORIENTED_EDGE('',*,*,#7095,.F.);
#9730=ORIENTED_EDGE('',*,*,#6881,.T.);
#9731=ORIENTED_EDGE('',*,*,#7097,.T.);
#9732=ORIENTED_EDGE('',*,*,#7084,.F.);
#9733=ORIENTED_EDGE('',*,*,#7112,.T.);
#9734=ORIENTED_EDGE('',*,*,#7113,.F.);
#9735=ORIENTED_EDGE('',*,*,#7082,.T.);
#9736=ORIENTED_EDGE('',*,*,#6936,.T.);
#9737=ORIENTED_EDGE('',*,*,#6911,.T.);
#9738=ORIENTED_EDGE('',*,*,#7113,.T.);
#9739=ORIENTED_EDGE('',*,*,#7111,.T.);
#9740=ORIENTED_EDGE('',*,*,#7109,.T.);
#9741=ORIENTED_EDGE('',*,*,#7107,.T.);
#9742=ORIENTED_EDGE('',*,*,#7105,.T.);
#9743=ORIENTED_EDGE('',*,*,#7103,.T.);
#9744=ORIENTED_EDGE('',*,*,#7101,.T.);
#9745=ORIENTED_EDGE('',*,*,#7066,.T.);
#9746=ORIENTED_EDGE('',*,*,#7071,.T.);
#9747=ORIENTED_EDGE('',*,*,#7075,.T.);
#9748=ORIENTED_EDGE('',*,*,#7077,.T.);
#9749=ORIENTED_EDGE('',*,*,#7079,.T.);
#9750=ORIENTED_EDGE('',*,*,#7081,.T.);
#9751=ORIENTED_EDGE('',*,*,#7083,.T.);
#9752=ORIENTED_EDGE('',*,*,#6883,.T.);
#9753=ORIENTED_EDGE('',*,*,#6910,.T.);
#9754=ORIENTED_EDGE('',*,*,#6935,.T.);
#9755=ORIENTED_EDGE('',*,*,#7114,.T.);
#9756=ORIENTED_EDGE('',*,*,#7115,.F.);
#9757=ORIENTED_EDGE('',*,*,#7116,.F.);
#9758=ORIENTED_EDGE('',*,*,#7117,.F.);
#9759=ORIENTED_EDGE('',*,*,#7118,.T.);
#9760=ORIENTED_EDGE('',*,*,#6934,.T.);
#9761=ORIENTED_EDGE('',*,*,#7119,.T.);
#9762=ORIENTED_EDGE('',*,*,#7120,.F.);
#9763=ORIENTED_EDGE('',*,*,#7114,.F.);
#9764=ORIENTED_EDGE('',*,*,#6884,.T.);
#9765=ORIENTED_EDGE('',*,*,#7118,.F.);
#9766=ORIENTED_EDGE('',*,*,#7121,.F.);
#9767=ORIENTED_EDGE('',*,*,#7122,.T.);
#9768=ORIENTED_EDGE('',*,*,#6933,.T.);
#9769=ORIENTED_EDGE('',*,*,#7123,.T.);
#9770=ORIENTED_EDGE('',*,*,#7124,.F.);
#9771=ORIENTED_EDGE('',*,*,#7119,.F.);
#9772=ORIENTED_EDGE('',*,*,#6932,.T.);
#9773=ORIENTED_EDGE('',*,*,#7125,.T.);
#9774=ORIENTED_EDGE('',*,*,#7126,.F.);
#9775=ORIENTED_EDGE('',*,*,#7123,.F.);
#9776=ORIENTED_EDGE('',*,*,#6931,.T.);
#9777=ORIENTED_EDGE('',*,*,#7127,.T.);
#9778=ORIENTED_EDGE('',*,*,#7128,.F.);
#9779=ORIENTED_EDGE('',*,*,#7125,.F.);
#9780=ORIENTED_EDGE('',*,*,#6930,.T.);
#9781=ORIENTED_EDGE('',*,*,#7129,.T.);
#9782=ORIENTED_EDGE('',*,*,#7130,.F.);
#9783=ORIENTED_EDGE('',*,*,#7127,.F.);
#9784=ORIENTED_EDGE('',*,*,#6929,.T.);
#9785=ORIENTED_EDGE('',*,*,#7131,.F.);
#9786=ORIENTED_EDGE('',*,*,#7132,.F.);
#9787=ORIENTED_EDGE('',*,*,#7129,.F.);
#9788=ORIENTED_EDGE('',*,*,#7133,.T.);
#9789=ORIENTED_EDGE('',*,*,#7134,.T.);
#9790=ORIENTED_EDGE('',*,*,#7135,.T.);
#9791=ORIENTED_EDGE('',*,*,#7136,.T.);
#9792=ORIENTED_EDGE('',*,*,#7137,.T.);
#9793=ORIENTED_EDGE('',*,*,#7138,.T.);
#9794=ORIENTED_EDGE('',*,*,#7121,.T.);
#9795=ORIENTED_EDGE('',*,*,#7117,.T.);
#9796=ORIENTED_EDGE('',*,*,#7139,.T.);
#9797=ORIENTED_EDGE('',*,*,#7140,.T.);
#9798=ORIENTED_EDGE('',*,*,#7141,.T.);
#9799=ORIENTED_EDGE('',*,*,#7142,.T.);
#9800=ORIENTED_EDGE('',*,*,#7143,.T.);
#9801=ORIENTED_EDGE('',*,*,#7144,.T.);
#9802=ORIENTED_EDGE('',*,*,#6889,.T.);
#9803=ORIENTED_EDGE('',*,*,#7145,.F.);
#9804=ORIENTED_EDGE('',*,*,#7134,.F.);
#9805=ORIENTED_EDGE('',*,*,#7146,.F.);
#9806=ORIENTED_EDGE('',*,*,#6888,.T.);
#9807=ORIENTED_EDGE('',*,*,#7147,.F.);
#9808=ORIENTED_EDGE('',*,*,#7135,.F.);
#9809=ORIENTED_EDGE('',*,*,#7145,.T.);
#9810=ORIENTED_EDGE('',*,*,#6887,.T.);
#9811=ORIENTED_EDGE('',*,*,#7148,.F.);
#9812=ORIENTED_EDGE('',*,*,#7136,.F.);
#9813=ORIENTED_EDGE('',*,*,#7147,.T.);
#9814=ORIENTED_EDGE('',*,*,#6886,.T.);
#9815=ORIENTED_EDGE('',*,*,#7149,.F.);
#9816=ORIENTED_EDGE('',*,*,#7137,.F.);
#9817=ORIENTED_EDGE('',*,*,#7148,.T.);
#9818=ORIENTED_EDGE('',*,*,#6885,.T.);
#9819=ORIENTED_EDGE('',*,*,#7122,.F.);
#9820=ORIENTED_EDGE('',*,*,#7138,.F.);
#9821=ORIENTED_EDGE('',*,*,#7149,.T.);
#9822=ORIENTED_EDGE('',*,*,#7116,.T.);
#9823=ORIENTED_EDGE('',*,*,#7150,.F.);
#9824=ORIENTED_EDGE('',*,*,#7151,.F.);
#9825=ORIENTED_EDGE('',*,*,#7139,.F.);
#9826=ORIENTED_EDGE('',*,*,#7151,.T.);
#9827=ORIENTED_EDGE('',*,*,#7152,.F.);
#9828=ORIENTED_EDGE('',*,*,#7153,.F.);
#9829=ORIENTED_EDGE('',*,*,#7140,.F.);
#9830=ORIENTED_EDGE('',*,*,#7153,.T.);
#9831=ORIENTED_EDGE('',*,*,#7154,.F.);
#9832=ORIENTED_EDGE('',*,*,#7155,.F.);
#9833=ORIENTED_EDGE('',*,*,#7141,.F.);
#9834=ORIENTED_EDGE('',*,*,#7155,.T.);
#9835=ORIENTED_EDGE('',*,*,#7156,.F.);
#9836=ORIENTED_EDGE('',*,*,#7157,.F.);
#9837=ORIENTED_EDGE('',*,*,#7142,.F.);
#9838=ORIENTED_EDGE('',*,*,#7157,.T.);
#9839=ORIENTED_EDGE('',*,*,#7158,.F.);
#9840=ORIENTED_EDGE('',*,*,#7159,.F.);
#9841=ORIENTED_EDGE('',*,*,#7143,.F.);
#9842=ORIENTED_EDGE('',*,*,#7159,.T.);
#9843=ORIENTED_EDGE('',*,*,#7160,.F.);
#9844=ORIENTED_EDGE('',*,*,#7161,.F.);
#9845=ORIENTED_EDGE('',*,*,#7144,.F.);
#9846=ORIENTED_EDGE('',*,*,#6890,.T.);
#9847=ORIENTED_EDGE('',*,*,#7146,.T.);
#9848=ORIENTED_EDGE('',*,*,#7133,.F.);
#9849=ORIENTED_EDGE('',*,*,#7161,.T.);
#9850=ORIENTED_EDGE('',*,*,#7162,.F.);
#9851=ORIENTED_EDGE('',*,*,#7131,.T.);
#9852=ORIENTED_EDGE('',*,*,#6928,.T.);
#9853=ORIENTED_EDGE('',*,*,#6901,.T.);
#9854=ORIENTED_EDGE('',*,*,#7162,.T.);
#9855=ORIENTED_EDGE('',*,*,#7160,.T.);
#9856=ORIENTED_EDGE('',*,*,#7158,.T.);
#9857=ORIENTED_EDGE('',*,*,#7156,.T.);
#9858=ORIENTED_EDGE('',*,*,#7154,.T.);
#9859=ORIENTED_EDGE('',*,*,#7152,.T.);
#9860=ORIENTED_EDGE('',*,*,#7150,.T.);
#9861=ORIENTED_EDGE('',*,*,#7115,.T.);
#9862=ORIENTED_EDGE('',*,*,#7120,.T.);
#9863=ORIENTED_EDGE('',*,*,#7124,.T.);
#9864=ORIENTED_EDGE('',*,*,#7126,.T.);
#9865=ORIENTED_EDGE('',*,*,#7128,.T.);
#9866=ORIENTED_EDGE('',*,*,#7130,.T.);
#9867=ORIENTED_EDGE('',*,*,#7132,.T.);
#9868=ORIENTED_EDGE('',*,*,#6865,.T.);
#9869=ORIENTED_EDGE('',*,*,#6913,.T.);
#9870=ORIENTED_EDGE('',*,*,#6951,.T.);
#9871=ORIENTED_EDGE('',*,*,#7163,.T.);
#9872=ORIENTED_EDGE('',*,*,#7164,.F.);
#9873=ORIENTED_EDGE('',*,*,#7165,.F.);
#9874=ORIENTED_EDGE('',*,*,#7166,.F.);
#9875=ORIENTED_EDGE('',*,*,#7167,.T.);
#9876=ORIENTED_EDGE('',*,*,#6950,.T.);
#9877=ORIENTED_EDGE('',*,*,#7168,.T.);
#9878=ORIENTED_EDGE('',*,*,#7169,.F.);
#9879=ORIENTED_EDGE('',*,*,#7163,.F.);
#9880=ORIENTED_EDGE('',*,*,#6866,.T.);
#9881=ORIENTED_EDGE('',*,*,#7167,.F.);
#9882=ORIENTED_EDGE('',*,*,#7170,.F.);
#9883=ORIENTED_EDGE('',*,*,#7171,.T.);
#9884=ORIENTED_EDGE('',*,*,#6949,.T.);
#9885=ORIENTED_EDGE('',*,*,#7172,.T.);
#9886=ORIENTED_EDGE('',*,*,#7173,.F.);
#9887=ORIENTED_EDGE('',*,*,#7168,.F.);
#9888=ORIENTED_EDGE('',*,*,#6948,.T.);
#9889=ORIENTED_EDGE('',*,*,#7174,.T.);
#9890=ORIENTED_EDGE('',*,*,#7175,.F.);
#9891=ORIENTED_EDGE('',*,*,#7172,.F.);
#9892=ORIENTED_EDGE('',*,*,#6947,.T.);
#9893=ORIENTED_EDGE('',*,*,#7176,.T.);
#9894=ORIENTED_EDGE('',*,*,#7177,.F.);
#9895=ORIENTED_EDGE('',*,*,#7174,.F.);
#9896=ORIENTED_EDGE('',*,*,#6946,.T.);
#9897=ORIENTED_EDGE('',*,*,#7178,.T.);
#9898=ORIENTED_EDGE('',*,*,#7179,.F.);
#9899=ORIENTED_EDGE('',*,*,#7176,.F.);
#9900=ORIENTED_EDGE('',*,*,#6945,.T.);
#9901=ORIENTED_EDGE('',*,*,#7180,.F.);
#9902=ORIENTED_EDGE('',*,*,#7181,.F.);
#9903=ORIENTED_EDGE('',*,*,#7178,.F.);
#9904=ORIENTED_EDGE('',*,*,#7182,.T.);
#9905=ORIENTED_EDGE('',*,*,#7183,.T.);
#9906=ORIENTED_EDGE('',*,*,#7184,.T.);
#9907=ORIENTED_EDGE('',*,*,#7185,.T.);
#9908=ORIENTED_EDGE('',*,*,#7186,.T.);
#9909=ORIENTED_EDGE('',*,*,#7187,.T.);
#9910=ORIENTED_EDGE('',*,*,#7170,.T.);
#9911=ORIENTED_EDGE('',*,*,#7166,.T.);
#9912=ORIENTED_EDGE('',*,*,#7188,.T.);
#9913=ORIENTED_EDGE('',*,*,#7189,.T.);
#9914=ORIENTED_EDGE('',*,*,#7190,.T.);
#9915=ORIENTED_EDGE('',*,*,#7191,.T.);
#9916=ORIENTED_EDGE('',*,*,#7192,.T.);
#9917=ORIENTED_EDGE('',*,*,#7193,.T.);
#9918=ORIENTED_EDGE('',*,*,#6871,.T.);
#9919=ORIENTED_EDGE('',*,*,#7194,.F.);
#9920=ORIENTED_EDGE('',*,*,#7183,.F.);
#9921=ORIENTED_EDGE('',*,*,#7195,.F.);
#9922=ORIENTED_EDGE('',*,*,#6870,.T.);
#9923=ORIENTED_EDGE('',*,*,#7196,.F.);
#9924=ORIENTED_EDGE('',*,*,#7184,.F.);
#9925=ORIENTED_EDGE('',*,*,#7194,.T.);
#9926=ORIENTED_EDGE('',*,*,#6869,.T.);
#9927=ORIENTED_EDGE('',*,*,#7197,.F.);
#9928=ORIENTED_EDGE('',*,*,#7185,.F.);
#9929=ORIENTED_EDGE('',*,*,#7196,.T.);
#9930=ORIENTED_EDGE('',*,*,#6868,.T.);
#9931=ORIENTED_EDGE('',*,*,#7198,.F.);
#9932=ORIENTED_EDGE('',*,*,#7186,.F.);
#9933=ORIENTED_EDGE('',*,*,#7197,.T.);
#9934=ORIENTED_EDGE('',*,*,#6867,.T.);
#9935=ORIENTED_EDGE('',*,*,#7171,.F.);
#9936=ORIENTED_EDGE('',*,*,#7187,.F.);
#9937=ORIENTED_EDGE('',*,*,#7198,.T.);
#9938=ORIENTED_EDGE('',*,*,#7165,.T.);
#9939=ORIENTED_EDGE('',*,*,#7199,.F.);
#9940=ORIENTED_EDGE('',*,*,#7200,.F.);
#9941=ORIENTED_EDGE('',*,*,#7188,.F.);
#9942=ORIENTED_EDGE('',*,*,#7200,.T.);
#9943=ORIENTED_EDGE('',*,*,#7201,.F.);
#9944=ORIENTED_EDGE('',*,*,#7202,.F.);
#9945=ORIENTED_EDGE('',*,*,#7189,.F.);
#9946=ORIENTED_EDGE('',*,*,#7202,.T.);
#9947=ORIENTED_EDGE('',*,*,#7203,.F.);
#9948=ORIENTED_EDGE('',*,*,#7204,.F.);
#9949=ORIENTED_EDGE('',*,*,#7190,.F.);
#9950=ORIENTED_EDGE('',*,*,#7204,.T.);
#9951=ORIENTED_EDGE('',*,*,#7205,.F.);
#9952=ORIENTED_EDGE('',*,*,#7206,.F.);
#9953=ORIENTED_EDGE('',*,*,#7191,.F.);
#9954=ORIENTED_EDGE('',*,*,#7206,.T.);
#9955=ORIENTED_EDGE('',*,*,#7207,.F.);
#9956=ORIENTED_EDGE('',*,*,#7208,.F.);
#9957=ORIENTED_EDGE('',*,*,#7192,.F.);
#9958=ORIENTED_EDGE('',*,*,#7208,.T.);
#9959=ORIENTED_EDGE('',*,*,#7209,.F.);
#9960=ORIENTED_EDGE('',*,*,#7210,.F.);
#9961=ORIENTED_EDGE('',*,*,#7193,.F.);
#9962=ORIENTED_EDGE('',*,*,#6872,.T.);
#9963=ORIENTED_EDGE('',*,*,#7195,.T.);
#9964=ORIENTED_EDGE('',*,*,#7182,.F.);
#9965=ORIENTED_EDGE('',*,*,#7210,.T.);
#9966=ORIENTED_EDGE('',*,*,#7211,.F.);
#9967=ORIENTED_EDGE('',*,*,#7180,.T.);
#9968=ORIENTED_EDGE('',*,*,#6944,.T.);
#9969=ORIENTED_EDGE('',*,*,#6907,.T.);
#9970=ORIENTED_EDGE('',*,*,#7211,.T.);
#9971=ORIENTED_EDGE('',*,*,#7209,.T.);
#9972=ORIENTED_EDGE('',*,*,#7207,.T.);
#9973=ORIENTED_EDGE('',*,*,#7205,.T.);
#9974=ORIENTED_EDGE('',*,*,#7203,.T.);
#9975=ORIENTED_EDGE('',*,*,#7201,.T.);
#9976=ORIENTED_EDGE('',*,*,#7199,.T.);
#9977=ORIENTED_EDGE('',*,*,#7164,.T.);
#9978=ORIENTED_EDGE('',*,*,#7169,.T.);
#9979=ORIENTED_EDGE('',*,*,#7173,.T.);
#9980=ORIENTED_EDGE('',*,*,#7175,.T.);
#9981=ORIENTED_EDGE('',*,*,#7177,.T.);
#9982=ORIENTED_EDGE('',*,*,#7179,.T.);
#9983=ORIENTED_EDGE('',*,*,#7181,.T.);
#9984=ORIENTED_EDGE('',*,*,#6847,.T.);
#9985=ORIENTED_EDGE('',*,*,#6916,.T.);
#9986=ORIENTED_EDGE('',*,*,#6919,.T.);
#9987=ORIENTED_EDGE('',*,*,#7212,.T.);
#9988=ORIENTED_EDGE('',*,*,#7213,.F.);
#9989=ORIENTED_EDGE('',*,*,#7214,.F.);
#9990=ORIENTED_EDGE('',*,*,#7215,.F.);
#9991=ORIENTED_EDGE('',*,*,#7216,.T.);
#9992=ORIENTED_EDGE('',*,*,#6966,.T.);
#9993=ORIENTED_EDGE('',*,*,#7217,.T.);
#9994=ORIENTED_EDGE('',*,*,#7218,.F.);
#9995=ORIENTED_EDGE('',*,*,#7212,.F.);
#9996=ORIENTED_EDGE('',*,*,#6848,.T.);
#9997=ORIENTED_EDGE('',*,*,#7216,.F.);
#9998=ORIENTED_EDGE('',*,*,#7219,.F.);
#9999=ORIENTED_EDGE('',*,*,#7220,.T.);
#10000=ORIENTED_EDGE('',*,*,#6965,.T.);
#10001=ORIENTED_EDGE('',*,*,#7221,.T.);
#10002=ORIENTED_EDGE('',*,*,#7222,.F.);
#10003=ORIENTED_EDGE('',*,*,#7217,.F.);
#10004=ORIENTED_EDGE('',*,*,#6964,.T.);
#10005=ORIENTED_EDGE('',*,*,#7223,.T.);
#10006=ORIENTED_EDGE('',*,*,#7224,.F.);
#10007=ORIENTED_EDGE('',*,*,#7221,.F.);
#10008=ORIENTED_EDGE('',*,*,#6963,.T.);
#10009=ORIENTED_EDGE('',*,*,#7225,.T.);
#10010=ORIENTED_EDGE('',*,*,#7226,.F.);
#10011=ORIENTED_EDGE('',*,*,#7223,.F.);
#10012=ORIENTED_EDGE('',*,*,#6962,.T.);
#10013=ORIENTED_EDGE('',*,*,#7227,.T.);
#10014=ORIENTED_EDGE('',*,*,#7228,.F.);
#10015=ORIENTED_EDGE('',*,*,#7225,.F.);
#10016=ORIENTED_EDGE('',*,*,#6961,.T.);
#10017=ORIENTED_EDGE('',*,*,#7229,.F.);
#10018=ORIENTED_EDGE('',*,*,#7230,.F.);
#10019=ORIENTED_EDGE('',*,*,#7227,.F.);
#10020=ORIENTED_EDGE('',*,*,#7231,.T.);
#10021=ORIENTED_EDGE('',*,*,#7232,.T.);
#10022=ORIENTED_EDGE('',*,*,#7233,.T.);
#10023=ORIENTED_EDGE('',*,*,#7234,.T.);
#10024=ORIENTED_EDGE('',*,*,#7235,.T.);
#10025=ORIENTED_EDGE('',*,*,#7236,.T.);
#10026=ORIENTED_EDGE('',*,*,#7219,.T.);
#10027=ORIENTED_EDGE('',*,*,#7215,.T.);
#10028=ORIENTED_EDGE('',*,*,#7237,.T.);
#10029=ORIENTED_EDGE('',*,*,#7238,.T.);
#10030=ORIENTED_EDGE('',*,*,#7239,.T.);
#10031=ORIENTED_EDGE('',*,*,#7240,.T.);
#10032=ORIENTED_EDGE('',*,*,#7241,.T.);
#10033=ORIENTED_EDGE('',*,*,#7242,.T.);
#10034=ORIENTED_EDGE('',*,*,#6853,.T.);
#10035=ORIENTED_EDGE('',*,*,#7243,.F.);
#10036=ORIENTED_EDGE('',*,*,#7232,.F.);
#10037=ORIENTED_EDGE('',*,*,#7244,.F.);
#10038=ORIENTED_EDGE('',*,*,#6852,.T.);
#10039=ORIENTED_EDGE('',*,*,#7245,.F.);
#10040=ORIENTED_EDGE('',*,*,#7233,.F.);
#10041=ORIENTED_EDGE('',*,*,#7243,.T.);
#10042=ORIENTED_EDGE('',*,*,#6851,.T.);
#10043=ORIENTED_EDGE('',*,*,#7246,.F.);
#10044=ORIENTED_EDGE('',*,*,#7234,.F.);
#10045=ORIENTED_EDGE('',*,*,#7245,.T.);
#10046=ORIENTED_EDGE('',*,*,#6850,.T.);
#10047=ORIENTED_EDGE('',*,*,#7247,.F.);
#10048=ORIENTED_EDGE('',*,*,#7235,.F.);
#10049=ORIENTED_EDGE('',*,*,#7246,.T.);
#10050=ORIENTED_EDGE('',*,*,#6849,.T.);
#10051=ORIENTED_EDGE('',*,*,#7220,.F.);
#10052=ORIENTED_EDGE('',*,*,#7236,.F.);
#10053=ORIENTED_EDGE('',*,*,#7247,.T.);
#10054=ORIENTED_EDGE('',*,*,#7214,.T.);
#10055=ORIENTED_EDGE('',*,*,#7248,.F.);
#10056=ORIENTED_EDGE('',*,*,#7249,.F.);
#10057=ORIENTED_EDGE('',*,*,#7237,.F.);
#10058=ORIENTED_EDGE('',*,*,#7249,.T.);
#10059=ORIENTED_EDGE('',*,*,#7250,.F.);
#10060=ORIENTED_EDGE('',*,*,#7251,.F.);
#10061=ORIENTED_EDGE('',*,*,#7238,.F.);
#10062=ORIENTED_EDGE('',*,*,#7251,.T.);
#10063=ORIENTED_EDGE('',*,*,#7252,.F.);
#10064=ORIENTED_EDGE('',*,*,#7253,.F.);
#10065=ORIENTED_EDGE('',*,*,#7239,.F.);
#10066=ORIENTED_EDGE('',*,*,#7253,.T.);
#10067=ORIENTED_EDGE('',*,*,#7254,.F.);
#10068=ORIENTED_EDGE('',*,*,#7255,.F.);
#10069=ORIENTED_EDGE('',*,*,#7240,.F.);
#10070=ORIENTED_EDGE('',*,*,#7255,.T.);
#10071=ORIENTED_EDGE('',*,*,#7256,.F.);
#10072=ORIENTED_EDGE('',*,*,#7257,.F.);
#10073=ORIENTED_EDGE('',*,*,#7241,.F.);
#10074=ORIENTED_EDGE('',*,*,#7257,.T.);
#10075=ORIENTED_EDGE('',*,*,#7258,.F.);
#10076=ORIENTED_EDGE('',*,*,#7259,.F.);
#10077=ORIENTED_EDGE('',*,*,#7242,.F.);
#10078=ORIENTED_EDGE('',*,*,#6854,.T.);
#10079=ORIENTED_EDGE('',*,*,#7244,.T.);
#10080=ORIENTED_EDGE('',*,*,#7231,.F.);
#10081=ORIENTED_EDGE('',*,*,#7259,.T.);
#10082=ORIENTED_EDGE('',*,*,#7260,.F.);
#10083=ORIENTED_EDGE('',*,*,#7229,.T.);
#10084=ORIENTED_EDGE('',*,*,#6960,.T.);
#10085=ORIENTED_EDGE('',*,*,#6904,.T.);
#10086=ORIENTED_EDGE('',*,*,#7260,.T.);
#10087=ORIENTED_EDGE('',*,*,#7258,.T.);
#10088=ORIENTED_EDGE('',*,*,#7256,.T.);
#10089=ORIENTED_EDGE('',*,*,#7254,.T.);
#10090=ORIENTED_EDGE('',*,*,#7252,.T.);
#10091=ORIENTED_EDGE('',*,*,#7250,.T.);
#10092=ORIENTED_EDGE('',*,*,#7248,.T.);
#10093=ORIENTED_EDGE('',*,*,#7213,.T.);
#10094=ORIENTED_EDGE('',*,*,#7218,.T.);
#10095=ORIENTED_EDGE('',*,*,#7222,.T.);
#10096=ORIENTED_EDGE('',*,*,#7224,.T.);
#10097=ORIENTED_EDGE('',*,*,#7226,.T.);
#10098=ORIENTED_EDGE('',*,*,#7228,.T.);
#10099=ORIENTED_EDGE('',*,*,#7230,.T.);
#10100=ORIENTED_EDGE('',*,*,#7261,.T.);
#10101=ORIENTED_EDGE('',*,*,#7262,.T.);
#10102=ORIENTED_EDGE('',*,*,#7263,.T.);
#10103=ORIENTED_EDGE('',*,*,#7264,.T.);
#10104=ORIENTED_EDGE('',*,*,#7265,.T.);
#10105=ORIENTED_EDGE('',*,*,#7266,.T.);
#10106=ORIENTED_EDGE('',*,*,#7261,.F.);
#10107=ORIENTED_EDGE('',*,*,#7267,.T.);
#10108=ORIENTED_EDGE('',*,*,#7268,.T.);
#10109=ORIENTED_EDGE('',*,*,#7269,.T.);
#10110=ORIENTED_EDGE('',*,*,#7265,.F.);
#10111=ORIENTED_EDGE('',*,*,#7270,.T.);
#10112=ORIENTED_EDGE('',*,*,#7263,.F.);
#10113=ORIENTED_EDGE('',*,*,#7271,.T.);
#10114=ORIENTED_EDGE('',*,*,#7268,.F.);
#10115=ORIENTED_EDGE('',*,*,#7272,.T.);
#10116=ORIENTED_EDGE('',*,*,#7267,.F.);
#10117=ORIENTED_EDGE('',*,*,#7273,.F.);
#10118=ORIENTED_EDGE('',*,*,#7274,.F.);
#10119=ORIENTED_EDGE('',*,*,#7275,.T.);
#10120=ORIENTED_EDGE('',*,*,#7264,.F.);
#10121=ORIENTED_EDGE('',*,*,#7276,.F.);
#10122=ORIENTED_EDGE('',*,*,#7277,.F.);
#10123=ORIENTED_EDGE('',*,*,#7273,.T.);
#10124=ORIENTED_EDGE('',*,*,#7262,.F.);
#10125=ORIENTED_EDGE('',*,*,#7266,.F.);
#10126=ORIENTED_EDGE('',*,*,#7269,.F.);
#10127=ORIENTED_EDGE('',*,*,#7271,.F.);
#10128=ORIENTED_EDGE('',*,*,#7278,.T.);
#10129=ORIENTED_EDGE('',*,*,#7277,.T.);
#10130=ORIENTED_EDGE('',*,*,#7279,.T.);
#10131=ORIENTED_EDGE('',*,*,#7280,.T.);
#10132=ORIENTED_EDGE('',*,*,#7281,.T.);
#10133=ORIENTED_EDGE('',*,*,#7274,.T.);
#10134=ORIENTED_EDGE('',*,*,#7278,.F.);
#10135=ORIENTED_EDGE('',*,*,#7282,.T.);
#10136=ORIENTED_EDGE('',*,*,#7283,.T.);
#10137=ORIENTED_EDGE('',*,*,#7284,.T.);
#10138=ORIENTED_EDGE('',*,*,#7281,.F.);
#10139=ORIENTED_EDGE('',*,*,#7285,.T.);
#10140=ORIENTED_EDGE('',*,*,#7279,.F.);
#10141=ORIENTED_EDGE('',*,*,#7286,.T.);
#10142=ORIENTED_EDGE('',*,*,#7283,.F.);
#10143=ORIENTED_EDGE('',*,*,#7287,.T.);
#10144=ORIENTED_EDGE('',*,*,#7272,.F.);
#10145=ORIENTED_EDGE('',*,*,#7288,.F.);
#10146=ORIENTED_EDGE('',*,*,#7286,.F.);
#10147=ORIENTED_EDGE('',*,*,#7276,.T.);
#10148=ORIENTED_EDGE('',*,*,#7280,.F.);
#10149=ORIENTED_EDGE('',*,*,#7287,.F.);
#10150=ORIENTED_EDGE('',*,*,#7285,.F.);
#10151=ORIENTED_EDGE('',*,*,#7282,.F.);
#10152=ORIENTED_EDGE('',*,*,#7270,.F.);
#10153=ORIENTED_EDGE('',*,*,#7275,.F.);
#10154=ORIENTED_EDGE('',*,*,#7284,.F.);
#10155=ORIENTED_EDGE('',*,*,#7288,.T.);
#10156=ORIENTED_EDGE('',*,*,#7289,.F.);
#10157=ORIENTED_EDGE('',*,*,#7290,.T.);
#10158=ORIENTED_EDGE('',*,*,#7291,.T.);
#10159=ORIENTED_EDGE('',*,*,#7292,.F.);
#10160=ORIENTED_EDGE('',*,*,#7293,.F.);
#10161=ORIENTED_EDGE('',*,*,#7294,.T.);
#10162=ORIENTED_EDGE('',*,*,#7295,.T.);
#10163=ORIENTED_EDGE('',*,*,#7290,.F.);
#10164=ORIENTED_EDGE('',*,*,#7296,.F.);
#10165=ORIENTED_EDGE('',*,*,#7297,.T.);
#10166=ORIENTED_EDGE('',*,*,#7298,.T.);
#10167=ORIENTED_EDGE('',*,*,#7294,.F.);
#10168=ORIENTED_EDGE('',*,*,#7299,.F.);
#10169=ORIENTED_EDGE('',*,*,#7300,.T.);
#10170=ORIENTED_EDGE('',*,*,#7301,.T.);
#10171=ORIENTED_EDGE('',*,*,#7297,.F.);
#10172=ORIENTED_EDGE('',*,*,#7302,.F.);
#10173=ORIENTED_EDGE('',*,*,#7303,.T.);
#10174=ORIENTED_EDGE('',*,*,#7304,.T.);
#10175=ORIENTED_EDGE('',*,*,#7300,.F.);
#10176=ORIENTED_EDGE('',*,*,#7305,.F.);
#10177=ORIENTED_EDGE('',*,*,#7292,.T.);
#10178=ORIENTED_EDGE('',*,*,#7306,.T.);
#10179=ORIENTED_EDGE('',*,*,#7303,.F.);
#10180=ORIENTED_EDGE('',*,*,#7306,.F.);
#10181=ORIENTED_EDGE('',*,*,#7291,.F.);
#10182=ORIENTED_EDGE('',*,*,#7295,.F.);
#10183=ORIENTED_EDGE('',*,*,#7298,.F.);
#10184=ORIENTED_EDGE('',*,*,#7301,.F.);
#10185=ORIENTED_EDGE('',*,*,#7304,.F.);
#10186=ORIENTED_EDGE('',*,*,#7307,.F.);
#10187=ORIENTED_EDGE('',*,*,#7289,.T.);
#10188=ORIENTED_EDGE('',*,*,#7305,.T.);
#10189=ORIENTED_EDGE('',*,*,#7302,.T.);
#10190=ORIENTED_EDGE('',*,*,#7299,.T.);
#10191=ORIENTED_EDGE('',*,*,#7296,.T.);
#10192=ORIENTED_EDGE('',*,*,#7293,.T.);
#10193=ORIENTED_EDGE('',*,*,#7308,.F.);
#10194=ORIENTED_EDGE('',*,*,#7309,.T.);
#10195=ORIENTED_EDGE('',*,*,#7307,.T.);
#10196=ORIENTED_EDGE('',*,*,#7309,.F.);
#10197=ORIENTED_EDGE('',*,*,#7310,.F.);
#10198=ORIENTED_EDGE('',*,*,#7311,.T.);
#10199=ORIENTED_EDGE('',*,*,#7308,.T.);
#10200=ORIENTED_EDGE('',*,*,#7311,.F.);
#10201=ORIENTED_EDGE('',*,*,#7312,.F.);
#10202=ORIENTED_EDGE('',*,*,#7313,.T.);
#10203=ORIENTED_EDGE('',*,*,#7310,.T.);
#10204=ORIENTED_EDGE('',*,*,#7313,.F.);
#10205=ORIENTED_EDGE('',*,*,#7312,.T.);
#10206=ORIENTED_EDGE('',*,*,#7314,.F.);
#10207=ORIENTED_EDGE('',*,*,#7315,.F.);
#10208=ORIENTED_EDGE('',*,*,#7316,.T.);
#10209=ORIENTED_EDGE('',*,*,#7314,.T.);
#10210=ORIENTED_EDGE('',*,*,#7316,.F.);
#10211=ORIENTED_EDGE('',*,*,#7317,.F.);
#10212=ORIENTED_EDGE('',*,*,#7318,.T.);
#10213=ORIENTED_EDGE('',*,*,#7315,.T.);
#10214=ORIENTED_EDGE('',*,*,#7318,.F.);
#10215=ORIENTED_EDGE('',*,*,#7319,.F.);
#10216=ORIENTED_EDGE('',*,*,#7320,.T.);
#10217=ORIENTED_EDGE('',*,*,#7317,.T.);
#10218=ORIENTED_EDGE('',*,*,#7320,.F.);
#10219=ORIENTED_EDGE('',*,*,#7319,.T.);
#10220=ORIENTED_EDGE('',*,*,#7321,.F.);
#10221=ORIENTED_EDGE('',*,*,#7322,.F.);
#10222=ORIENTED_EDGE('',*,*,#7323,.T.);
#10223=ORIENTED_EDGE('',*,*,#7321,.T.);
#10224=ORIENTED_EDGE('',*,*,#7323,.F.);
#10225=ORIENTED_EDGE('',*,*,#7324,.F.);
#10226=ORIENTED_EDGE('',*,*,#7325,.T.);
#10227=ORIENTED_EDGE('',*,*,#7322,.T.);
#10228=ORIENTED_EDGE('',*,*,#7325,.F.);
#10229=ORIENTED_EDGE('',*,*,#7326,.F.);
#10230=ORIENTED_EDGE('',*,*,#7327,.T.);
#10231=ORIENTED_EDGE('',*,*,#7324,.T.);
#10232=ORIENTED_EDGE('',*,*,#7327,.F.);
#10233=ORIENTED_EDGE('',*,*,#7326,.T.);
#10234=ORIENTED_EDGE('',*,*,#7328,.T.);
#10235=ORIENTED_EDGE('',*,*,#7329,.T.);
#10236=ORIENTED_EDGE('',*,*,#7330,.T.);
#10237=ORIENTED_EDGE('',*,*,#7331,.F.);
#10238=ORIENTED_EDGE('',*,*,#7332,.T.);
#10239=ORIENTED_EDGE('',*,*,#7333,.T.);
#10240=ORIENTED_EDGE('',*,*,#7334,.T.);
#10241=ORIENTED_EDGE('',*,*,#7329,.F.);
#10242=ORIENTED_EDGE('',*,*,#7335,.T.);
#10243=ORIENTED_EDGE('',*,*,#7336,.T.);
#10244=ORIENTED_EDGE('',*,*,#7337,.T.);
#10245=ORIENTED_EDGE('',*,*,#7333,.F.);
#10246=ORIENTED_EDGE('',*,*,#7338,.T.);
#10247=ORIENTED_EDGE('',*,*,#7339,.T.);
#10248=ORIENTED_EDGE('',*,*,#7340,.T.);
#10249=ORIENTED_EDGE('',*,*,#7336,.F.);
#10250=ORIENTED_EDGE('',*,*,#7341,.T.);
#10251=ORIENTED_EDGE('',*,*,#7342,.T.);
#10252=ORIENTED_EDGE('',*,*,#7343,.T.);
#10253=ORIENTED_EDGE('',*,*,#7339,.F.);
#10254=ORIENTED_EDGE('',*,*,#7344,.T.);
#10255=ORIENTED_EDGE('',*,*,#7331,.T.);
#10256=ORIENTED_EDGE('',*,*,#7345,.T.);
#10257=ORIENTED_EDGE('',*,*,#7342,.F.);
#10258=ORIENTED_EDGE('',*,*,#7344,.F.);
#10259=ORIENTED_EDGE('',*,*,#7341,.F.);
#10260=ORIENTED_EDGE('',*,*,#7338,.F.);
#10261=ORIENTED_EDGE('',*,*,#7335,.F.);
#10262=ORIENTED_EDGE('',*,*,#7332,.F.);
#10263=ORIENTED_EDGE('',*,*,#7328,.F.);
#10264=ORIENTED_EDGE('',*,*,#7345,.F.);
#10265=ORIENTED_EDGE('',*,*,#7330,.F.);
#10266=ORIENTED_EDGE('',*,*,#7334,.F.);
#10267=ORIENTED_EDGE('',*,*,#7337,.F.);
#10268=ORIENTED_EDGE('',*,*,#7340,.F.);
#10269=ORIENTED_EDGE('',*,*,#7343,.F.);
#10270=CYLINDRICAL_SURFACE('',#11376,0.21);
#10271=CYLINDRICAL_SURFACE('',#11379,0.21);
#10272=CYLINDRICAL_SURFACE('',#11382,0.34);
#10273=CYLINDRICAL_SURFACE('',#11385,0.34);
#10274=CYLINDRICAL_SURFACE('',#11388,0.34);
#10275=CYLINDRICAL_SURFACE('',#11391,0.34);
#10276=CYLINDRICAL_SURFACE('',#11415,0.425);
#10277=CYLINDRICAL_SURFACE('',#11418,0.645);
#10278=CYLINDRICAL_SURFACE('',#11424,0.425);
#10279=CYLINDRICAL_SURFACE('',#11427,0.645);
#10280=CYLINDRICAL_SURFACE('',#11433,0.425);
#10281=CYLINDRICAL_SURFACE('',#11436,0.645);
#10282=CYLINDRICAL_SURFACE('',#11442,0.425);
#10283=CYLINDRICAL_SURFACE('',#11445,0.645);
#10284=CYLINDRICAL_SURFACE('',#11451,0.17);
#10285=CYLINDRICAL_SURFACE('',#11454,0.17);
#10286=CYLINDRICAL_SURFACE('',#11457,0.17);
#10287=CYLINDRICAL_SURFACE('',#11460,0.17);
#10288=CYLINDRICAL_SURFACE('',#11463,1.11);
#10289=CYLINDRICAL_SURFACE('',#11466,0.275);
#10290=CYLINDRICAL_SURFACE('',#11469,0.275);
#10291=CYLINDRICAL_SURFACE('',#11481,0.125);
#10292=CYLINDRICAL_SURFACE('',#11485,0.125);
#10293=CYLINDRICAL_SURFACE('',#11489,0.125);
#10294=CYLINDRICAL_SURFACE('',#11493,0.125);
#10295=CYLINDRICAL_SURFACE('',#11497,1.1);
#10296=CYLINDRICAL_SURFACE('',#11502,0.26);
#10297=CYLINDRICAL_SURFACE('',#11521,0.275);
#10298=CYLINDRICAL_SURFACE('',#11524,0.15);
#10299=CYLINDRICAL_SURFACE('',#11538,0.275);
#10300=CYLINDRICAL_SURFACE('',#11541,0.15);
#10301=CYLINDRICAL_SURFACE('',#11555,0.275);
#10302=CYLINDRICAL_SURFACE('',#11558,0.15);
#10303=CYLINDRICAL_SURFACE('',#11572,0.275);
#10304=CYLINDRICAL_SURFACE('',#11575,0.15);
#10305=CYLINDRICAL_SURFACE('',#11582,2.05);
#10306=CYLINDRICAL_SURFACE('',#11587,2.05);
#10307=CYLINDRICAL_SURFACE('',#11609,2.8);
#10308=CYLINDRICAL_SURFACE('',#11612,2.8);
#10309=CYLINDRICAL_SURFACE('',#11621,0.65);
#10310=CYLINDRICAL_SURFACE('',#11623,0.65);
#10311=CYLINDRICAL_SURFACE('',#11631,1.8);
#10312=CYLINDRICAL_SURFACE('',#11640,0.25);
#10313=CYLINDRICAL_SURFACE('',#11641,0.25);
#10314=CYLINDRICAL_SURFACE('',#11642,1.65);
#10315=CYLINDRICAL_SURFACE('',#11645,0.25);
#10316=CYLINDRICAL_SURFACE('',#11646,0.25);
#10317=CYLINDRICAL_SURFACE('',#11647,0.25);
#10318=CYLINDRICAL_SURFACE('',#11648,0.25);
#10319=CYLINDRICAL_SURFACE('',#11653,1.75);
#10320=CYLINDRICAL_SURFACE('',#11657,0.6);
#10321=CYLINDRICAL_SURFACE('',#11661,0.42);
#10322=CYLINDRICAL_SURFACE('',#11664,0.8);
#10323=CYLINDRICAL_SURFACE('',#11684,0.65);
#10324=CYLINDRICAL_SURFACE('',#11692,0.3933);
#10325=CYLINDRICAL_SURFACE('',#11708,0.425);
#10326=CYLINDRICAL_SURFACE('',#11716,0.24505);
#10327=CYLINDRICAL_SURFACE('',#11751,0.165);
#10328=CYLINDRICAL_SURFACE('',#11755,0.6);
#10329=CYLINDRICAL_SURFACE('',#11761,0.25);
#10330=CYLINDRICAL_SURFACE('',#11769,0.165);
#10331=CYLINDRICAL_SURFACE('',#11773,0.25);
#10332=CYLINDRICAL_SURFACE('',#11776,0.6);
#10333=CYLINDRICAL_SURFACE('',#11784,0.21);
#10334=CYLINDRICAL_SURFACE('',#11794,0.6);
#10335=CYLINDRICAL_SURFACE('',#11802,2.8);
#10336=CYLINDRICAL_SURFACE('',#11803,1.2);
#10337=CYLINDRICAL_SURFACE('',#11805,1.2);
#10338=CYLINDRICAL_SURFACE('',#11810,0.21);
#10339=CYLINDRICAL_SURFACE('',#11814,0.605);
#10340=CYLINDRICAL_SURFACE('',#11817,1.1);
#10341=CYLINDRICAL_SURFACE('',#11825,0.21);
#10342=CYLINDRICAL_SURFACE('',#11829,0.605);
#10343=CYLINDRICAL_SURFACE('',#11832,1.1);
#10344=CYLINDRICAL_SURFACE('',#11838,0.225);
#10345=CYLINDRICAL_SURFACE('',#11841,0.8);
#10346=CYLINDRICAL_SURFACE('',#11858,0.1954);
#10347=CYLINDRICAL_SURFACE('',#11865,0.21);
#10348=CYLINDRICAL_SURFACE('',#11866,0.6);
#10349=CYLINDRICAL_SURFACE('',#11979,1.37);
#10350=CYLINDRICAL_SURFACE('',#11983,0.21);
#10351=CYLINDRICAL_SURFACE('',#11984,0.6);
#10352=CYLINDRICAL_SURFACE('',#12097,1.37);
#10353=CYLINDRICAL_SURFACE('',#12108,0.817);
#10354=CYLINDRICAL_SURFACE('',#12110,0.817);
#10355=CYLINDRICAL_SURFACE('',#12112,0.817);
#10356=CYLINDRICAL_SURFACE('',#12114,0.817);
#10357=CYLINDRICAL_SURFACE('',#12116,0.817);
#10358=CYLINDRICAL_SURFACE('',#12118,0.817);
#10359=CYLINDRICAL_SURFACE('',#12265,0.2);
#10360=CYLINDRICAL_SURFACE('',#12276,0.2);
#10361=CYLINDRICAL_SURFACE('',#12291,0.24505);
#10362=CYLINDRICAL_SURFACE('',#12301,0.35);
#10363=CYLINDRICAL_SURFACE('',#12309,0.1954);
#10364=ADVANCED_FACE('',(#1022),#10270,.F.);
#10365=ADVANCED_FACE('',(#1023),#10271,.F.);
#10366=ADVANCED_FACE('',(#1024),#10272,.F.);
#10367=ADVANCED_FACE('',(#1025),#10273,.F.);
#10368=ADVANCED_FACE('',(#1026),#10274,.F.);
#10369=ADVANCED_FACE('',(#1027),#10275,.F.);
#10370=ADVANCED_FACE('',(#1028),#516,.T.);
#10371=ADVANCED_FACE('',(#1029),#517,.T.);
#10372=ADVANCED_FACE('',(#1030),#518,.T.);
#10373=ADVANCED_FACE('',(#1031),#519,.T.);
#10374=ADVANCED_FACE('',(#1032,#403,#404,#405,#406,#407,#408),#520,.T.);
#10375=ADVANCED_FACE('',(#1033,#409,#410,#411,#412,#413,#414),#521,.F.);
#10376=ADVANCED_FACE('',(#1034),#522,.T.);
#10377=ADVANCED_FACE('',(#1035),#523,.T.);
#10378=ADVANCED_FACE('',(#1036),#524,.T.);
#10379=ADVANCED_FACE('',(#1037),#525,.T.);
#10380=ADVANCED_FACE('',(#1038),#526,.T.);
#10381=ADVANCED_FACE('',(#1039),#527,.F.);
#10382=ADVANCED_FACE('',(#1040),#528,.T.);
#10383=ADVANCED_FACE('',(#1041),#529,.T.);
#10384=ADVANCED_FACE('',(#1042),#530,.T.);
#10385=ADVANCED_FACE('',(#1043),#531,.T.);
#10386=ADVANCED_FACE('',(#1044),#532,.T.);
#10387=ADVANCED_FACE('',(#1045),#533,.F.);
#10388=ADVANCED_FACE('',(#1046),#10276,.F.);
#10389=ADVANCED_FACE('',(#1047),#10277,.T.);
#10390=ADVANCED_FACE('',(#1048,#415),#534,.T.);
#10391=ADVANCED_FACE('',(#1049,#416),#535,.F.);
#10392=ADVANCED_FACE('',(#1050),#10278,.F.);
#10393=ADVANCED_FACE('',(#1051),#10279,.T.);
#10394=ADVANCED_FACE('',(#1052,#417),#536,.T.);
#10395=ADVANCED_FACE('',(#1053,#418),#537,.F.);
#10396=ADVANCED_FACE('',(#1054),#10280,.F.);
#10397=ADVANCED_FACE('',(#1055),#10281,.T.);
#10398=ADVANCED_FACE('',(#1056,#419),#538,.T.);
#10399=ADVANCED_FACE('',(#1057,#420),#539,.F.);
#10400=ADVANCED_FACE('',(#1058),#10282,.F.);
#10401=ADVANCED_FACE('',(#1059),#10283,.T.);
#10402=ADVANCED_FACE('',(#1060,#421),#540,.T.);
#10403=ADVANCED_FACE('',(#1061,#422),#541,.F.);
#10404=ADVANCED_FACE('',(#1062),#10284,.F.);
#10405=ADVANCED_FACE('',(#1063),#10285,.F.);
#10406=ADVANCED_FACE('',(#1064),#10286,.F.);
#10407=ADVANCED_FACE('',(#1065),#10287,.F.);
#10408=ADVANCED_FACE('',(#1066),#10288,.F.);
#10409=ADVANCED_FACE('',(#1067),#10289,.F.);
#10410=ADVANCED_FACE('',(#1068),#10290,.F.);
#10411=ADVANCED_FACE('',(#1069,#423,#424),#542,.T.);
#10412=ADVANCED_FACE('',(#1070),#543,.F.);
#10413=ADVANCED_FACE('',(#1071,#425,#426,#427,#428,#429),#544,.T.);
#10414=ADVANCED_FACE('',(#1072),#545,.T.);
#10415=ADVANCED_FACE('',(#1073),#546,.T.);
#10416=ADVANCED_FACE('',(#1074,#430,#431,#432,#433,#434),#547,.T.);
#10417=ADVANCED_FACE('',(#1075),#548,.T.);
#10418=ADVANCED_FACE('',(#1076,#435,#436),#549,.F.);
#10419=ADVANCED_FACE('',(#1077),#10291,.F.);
#10420=ADVANCED_FACE('',(#1078),#550,.T.);
#10421=ADVANCED_FACE('',(#1079),#10292,.F.);
#10422=ADVANCED_FACE('',(#1080),#551,.T.);
#10423=ADVANCED_FACE('',(#1081),#10293,.F.);
#10424=ADVANCED_FACE('',(#1082),#552,.T.);
#10425=ADVANCED_FACE('',(#1083),#10294,.F.);
#10426=ADVANCED_FACE('',(#1084),#553,.T.);
#10427=ADVANCED_FACE('',(#1085),#10295,.T.);
#10428=ADVANCED_FACE('',(#1086,#437),#554,.T.);
#10429=ADVANCED_FACE('',(#1087),#10296,.F.);
#10430=ADVANCED_FACE('',(#1088,#438,#439,#440,#441,#442),#555,.T.);
#10431=ADVANCED_FACE('',(#1089),#556,.T.);
#10432=ADVANCED_FACE('',(#1090,#443),#557,.T.);
#10433=ADVANCED_FACE('',(#1091),#558,.T.);
#10434=ADVANCED_FACE('',(#1092),#559,.T.);
#10435=ADVANCED_FACE('',(#1093),#560,.F.);
#10436=ADVANCED_FACE('',(#1094),#561,.F.);
#10437=ADVANCED_FACE('',(#1095),#562,.F.);
#10438=ADVANCED_FACE('',(#1096),#563,.F.);
#10439=ADVANCED_FACE('',(#1097),#564,.F.);
#10440=ADVANCED_FACE('',(#1098),#565,.F.);
#10441=ADVANCED_FACE('',(#1099),#566,.F.);
#10442=ADVANCED_FACE('',(#1100),#567,.T.);
#10443=ADVANCED_FACE('',(#1101,#444),#568,.F.);
#10444=ADVANCED_FACE('',(#1102),#10297,.T.);
#10445=ADVANCED_FACE('',(#1103,#445),#569,.T.);
#10446=ADVANCED_FACE('',(#1104),#10298,.T.);
#10447=ADVANCED_FACE('',(#1105),#570,.F.);
#10448=ADVANCED_FACE('',(#1106),#571,.F.);
#10449=ADVANCED_FACE('',(#1107),#572,.F.);
#10450=ADVANCED_FACE('',(#1108),#573,.F.);
#10451=ADVANCED_FACE('',(#1109),#574,.F.);
#10452=ADVANCED_FACE('',(#1110),#575,.F.);
#10453=ADVANCED_FACE('',(#1111),#576,.F.);
#10454=ADVANCED_FACE('',(#1112),#577,.T.);
#10455=ADVANCED_FACE('',(#1113,#446),#578,.F.);
#10456=ADVANCED_FACE('',(#1114),#10299,.T.);
#10457=ADVANCED_FACE('',(#1115,#447),#579,.T.);
#10458=ADVANCED_FACE('',(#1116),#10300,.T.);
#10459=ADVANCED_FACE('',(#1117),#580,.F.);
#10460=ADVANCED_FACE('',(#1118),#581,.F.);
#10461=ADVANCED_FACE('',(#1119),#582,.F.);
#10462=ADVANCED_FACE('',(#1120),#583,.F.);
#10463=ADVANCED_FACE('',(#1121),#584,.F.);
#10464=ADVANCED_FACE('',(#1122),#585,.F.);
#10465=ADVANCED_FACE('',(#1123),#586,.F.);
#10466=ADVANCED_FACE('',(#1124),#587,.T.);
#10467=ADVANCED_FACE('',(#1125,#448),#588,.F.);
#10468=ADVANCED_FACE('',(#1126),#10301,.T.);
#10469=ADVANCED_FACE('',(#1127,#449),#589,.T.);
#10470=ADVANCED_FACE('',(#1128),#10302,.T.);
#10471=ADVANCED_FACE('',(#1129),#590,.F.);
#10472=ADVANCED_FACE('',(#1130),#591,.F.);
#10473=ADVANCED_FACE('',(#1131),#592,.F.);
#10474=ADVANCED_FACE('',(#1132),#593,.F.);
#10475=ADVANCED_FACE('',(#1133),#594,.F.);
#10476=ADVANCED_FACE('',(#1134),#595,.F.);
#10477=ADVANCED_FACE('',(#1135),#596,.F.);
#10478=ADVANCED_FACE('',(#1136),#597,.T.);
#10479=ADVANCED_FACE('',(#1137,#450),#598,.F.);
#10480=ADVANCED_FACE('',(#1138),#10303,.T.);
#10481=ADVANCED_FACE('',(#1139,#451),#599,.T.);
#10482=ADVANCED_FACE('',(#1140),#10304,.T.);
#10483=ADVANCED_FACE('',(#1141),#600,.F.);
#10484=ADVANCED_FACE('',(#1142),#601,.F.);
#10485=ADVANCED_FACE('',(#1143),#10305,.F.);
#10486=ADVANCED_FACE('',(#1144),#10306,.F.);
#10487=ADVANCED_FACE('',(#1145),#602,.T.);
#10488=ADVANCED_FACE('',(#1146),#603,.F.);
#10489=ADVANCED_FACE('',(#1147,#452,#453),#274,.F.);
#10490=ADVANCED_FACE('',(#1148),#604,.T.);
#10491=ADVANCED_FACE('',(#1149),#605,.T.);
#10492=ADVANCED_FACE('',(#1150),#606,.T.);
#10493=ADVANCED_FACE('',(#1151),#607,.T.);
#10494=ADVANCED_FACE('',(#1152),#608,.T.);
#10495=ADVANCED_FACE('',(#1153),#609,.T.);
#10496=ADVANCED_FACE('',(#1154,#454,#455,#456),#610,.T.);
#10497=ADVANCED_FACE('',(#1155),#10307,.T.);
#10498=ADVANCED_FACE('',(#1156),#10308,.T.);
#10499=ADVANCED_FACE('',(#1157),#611,.T.);
#10500=ADVANCED_FACE('',(#1158),#612,.F.);
#10501=ADVANCED_FACE('',(#1159),#613,.F.);
#10502=ADVANCED_FACE('',(#1160),#614,.F.);
#10503=ADVANCED_FACE('',(#1161),#615,.F.);
#10504=ADVANCED_FACE('',(#1162),#616,.F.);
#10505=ADVANCED_FACE('',(#1163),#617,.F.);
#10506=ADVANCED_FACE('',(#1164),#10309,.F.);
#10507=ADVANCED_FACE('',(#1165),#10310,.F.);
#10508=ADVANCED_FACE('',(#1166),#618,.T.);
#10509=ADVANCED_FACE('',(#1167),#619,.T.);
#10510=ADVANCED_FACE('',(#1168),#620,.T.);
#10511=ADVANCED_FACE('',(#1169),#621,.T.);
#10512=ADVANCED_FACE('',(#1170,#457,#458,#459),#622,.F.);
#10513=ADVANCED_FACE('',(#1171),#10311,.F.);
#10514=ADVANCED_FACE('',(#1172,#460),#623,.T.);
#10515=ADVANCED_FACE('',(#1173,#461,#462),#275,.T.);
#10516=ADVANCED_FACE('',(#1174,#463),#624,.T.);
#10517=ADVANCED_FACE('',(#1175),#10312,.F.);
#10518=ADVANCED_FACE('',(#1176),#10313,.F.);
#10519=ADVANCED_FACE('',(#1177,#464,#465,#466,#467,#468,#469),#10314,.T.);
#10520=ADVANCED_FACE('',(#1178),#10315,.F.);
#10521=ADVANCED_FACE('',(#1179),#10316,.F.);
#10522=ADVANCED_FACE('',(#1180),#10317,.F.);
#10523=ADVANCED_FACE('',(#1181),#10318,.F.);
#10524=ADVANCED_FACE('',(#1182,#470),#625,.T.);
#10525=ADVANCED_FACE('',(#1183,#471),#626,.T.);
#10526=ADVANCED_FACE('',(#1184),#10319,.T.);
#10527=ADVANCED_FACE('',(#1185,#472),#627,.T.);
#10528=ADVANCED_FACE('',(#1186,#473,#474,#475,#476,#477,#478),#10320,.F.);
#10529=ADVANCED_FACE('',(#1187),#10321,.F.);
#10530=ADVANCED_FACE('',(#1188),#10322,.T.);
#10531=ADVANCED_FACE('',(#1189,#479),#628,.T.);
#10532=ADVANCED_FACE('',(#1190,#480),#629,.F.);
#10533=ADVANCED_FACE('',(#1191),#630,.F.);
#10534=ADVANCED_FACE('',(#1192),#631,.F.);
#10535=ADVANCED_FACE('',(#1193),#632,.F.);
#10536=ADVANCED_FACE('',(#1194),#633,.F.);
#10537=ADVANCED_FACE('',(#1195),#634,.F.);
#10538=ADVANCED_FACE('',(#1196),#635,.F.);
#10539=ADVANCED_FACE('',(#1197),#636,.F.);
#10540=ADVANCED_FACE('',(#1198),#637,.F.);
#10541=ADVANCED_FACE('',(#1199),#638,.F.);
#10542=ADVANCED_FACE('',(#1200),#639,.T.);
#10543=ADVANCED_FACE('',(#1201),#11,.T.);
#10544=ADVANCED_FACE('',(#1202),#10323,.T.);
#10545=ADVANCED_FACE('',(#1203),#12,.T.);
#10546=ADVANCED_FACE('',(#1204,#481),#640,.T.);
#10547=ADVANCED_FACE('',(#1205),#13,.T.);
#10548=ADVANCED_FACE('',(#1206),#10324,.T.);
#10549=ADVANCED_FACE('',(#1207),#641,.F.);
#10550=ADVANCED_FACE('',(#1208),#642,.F.);
#10551=ADVANCED_FACE('',(#1209),#643,.F.);
#10552=ADVANCED_FACE('',(#1210),#644,.F.);
#10553=ADVANCED_FACE('',(#1211),#645,.F.);
#10554=ADVANCED_FACE('',(#1212),#646,.F.);
#10555=ADVANCED_FACE('',(#1213),#647,.F.);
#10556=ADVANCED_FACE('',(#1214),#648,.F.);
#10557=ADVANCED_FACE('',(#1215),#649,.F.);
#10558=ADVANCED_FACE('',(#1216),#650,.T.);
#10559=ADVANCED_FACE('',(#1217),#14,.T.);
#10560=ADVANCED_FACE('',(#1218),#10325,.T.);
#10561=ADVANCED_FACE('',(#1219),#15,.T.);
#10562=ADVANCED_FACE('',(#1220,#482),#651,.T.);
#10563=ADVANCED_FACE('',(#1221),#16,.T.);
#10564=ADVANCED_FACE('',(#1222),#10326,.T.);
#10565=ADVANCED_FACE('',(#1223),#652,.F.);
#10566=ADVANCED_FACE('',(#1224),#653,.T.);
#10567=ADVANCED_FACE('',(#1225),#654,.F.);
#10568=ADVANCED_FACE('',(#1226),#655,.F.);
#10569=ADVANCED_FACE('',(#1227),#656,.F.);
#10570=ADVANCED_FACE('',(#1228),#10327,.F.);
#10571=ADVANCED_FACE('',(#1229),#657,.T.);
#10572=ADVANCED_FACE('',(#1230,#483),#10328,.T.);
#10573=ADVANCED_FACE('',(#1231,#484),#658,.T.);
#10574=ADVANCED_FACE('',(#1232),#659,.F.);
#10575=ADVANCED_FACE('',(#1233),#10329,.T.);
#10576=ADVANCED_FACE('',(#1234),#660,.T.);
#10577=ADVANCED_FACE('',(#1235),#661,.F.);
#10578=ADVANCED_FACE('',(#1236),#662,.T.);
#10579=ADVANCED_FACE('',(#1237),#10330,.F.);
#10580=ADVANCED_FACE('',(#1238),#663,.T.);
#10581=ADVANCED_FACE('',(#1239,#485),#10331,.F.);
#10582=ADVANCED_FACE('',(#1240,#486),#10332,.T.);
#10583=ADVANCED_FACE('',(#1241,#487),#664,.T.);
#10584=ADVANCED_FACE('',(#1242,#488),#665,.F.);
#10585=ADVANCED_FACE('',(#1243),#666,.T.);
#10586=ADVANCED_FACE('',(#1244),#10333,.F.);
#10587=ADVANCED_FACE('',(#1245),#667,.T.);
#10588=ADVANCED_FACE('',(#1246),#668,.F.);
#10589=ADVANCED_FACE('',(#1247),#669,.F.);
#10590=ADVANCED_FACE('',(#1248),#670,.F.);
#10591=ADVANCED_FACE('',(#1249,#489),#671,.T.);
#10592=ADVANCED_FACE('',(#1250,#490),#10334,.F.);
#10593=ADVANCED_FACE('',(#1251,#491),#672,.T.);
#10594=ADVANCED_FACE('',(#1252,#492),#673,.F.);
#10595=ADVANCED_FACE('',(#1253),#10335,.T.);
#10596=ADVANCED_FACE('',(#1254,#493),#10336,.T.);
#10597=ADVANCED_FACE('',(#1255),#10337,.T.);
#10598=ADVANCED_FACE('',(#1256,#494),#674,.F.);
#10599=ADVANCED_FACE('',(#1257),#675,.T.);
#10600=ADVANCED_FACE('',(#1258),#10338,.F.);
#10601=ADVANCED_FACE('',(#1259),#676,.T.);
#10602=ADVANCED_FACE('',(#1260,#495),#10339,.F.);
#10603=ADVANCED_FACE('',(#1261,#496),#10340,.T.);
#10604=ADVANCED_FACE('',(#1262,#497),#677,.T.);
#10605=ADVANCED_FACE('',(#1263,#498),#678,.F.);
#10606=ADVANCED_FACE('',(#1264),#679,.T.);
#10607=ADVANCED_FACE('',(#1265),#10341,.F.);
#10608=ADVANCED_FACE('',(#1266),#680,.T.);
#10609=ADVANCED_FACE('',(#1267,#499),#10342,.F.);
#10610=ADVANCED_FACE('',(#1268,#500),#10343,.T.);
#10611=ADVANCED_FACE('',(#1269,#501),#681,.T.);
#10612=ADVANCED_FACE('',(#1270,#502),#682,.F.);
#10613=ADVANCED_FACE('',(#1271),#10344,.F.);
#10614=ADVANCED_FACE('',(#1272),#10345,.T.);
#10615=ADVANCED_FACE('',(#1273,#503),#683,.T.);
#10616=ADVANCED_FACE('',(#1274,#504),#684,.F.);
#10617=ADVANCED_FACE('',(#1275),#685,.F.);
#10618=ADVANCED_FACE('',(#1276),#686,.F.);
#10619=ADVANCED_FACE('',(#1277),#687,.F.);
#10620=ADVANCED_FACE('',(#1278),#688,.F.);
#10621=ADVANCED_FACE('',(#1279),#689,.F.);
#10622=ADVANCED_FACE('',(#1280),#690,.F.);
#10623=ADVANCED_FACE('',(#1281),#691,.F.);
#10624=ADVANCED_FACE('',(#1282,#505),#692,.T.);
#10625=ADVANCED_FACE('',(#1283),#17,.T.);
#10626=ADVANCED_FACE('',(#1284),#10346,.T.);
#10627=ADVANCED_FACE('',(#1285),#18,.T.);
#10628=ADVANCED_FACE('',(#1286),#693,.T.);
#10629=ADVANCED_FACE('',(#1287),#10347,.F.);
#10630=ADVANCED_FACE('',(#1288,#506),#10348,.F.);
#10631=ADVANCED_FACE('',(#1289),#694,.T.);
#10632=ADVANCED_FACE('',(#1290),#695,.T.);
#10633=ADVANCED_FACE('',(#1291),#696,.T.);
#10634=ADVANCED_FACE('',(#1292),#697,.T.);
#10635=ADVANCED_FACE('',(#1293),#698,.T.);
#10636=ADVANCED_FACE('',(#1294),#699,.T.);
#10637=ADVANCED_FACE('',(#1295),#700,.T.);
#10638=ADVANCED_FACE('',(#1296),#701,.T.);
#10639=ADVANCED_FACE('',(#1297),#702,.T.);
#10640=ADVANCED_FACE('',(#1298),#703,.T.);
#10641=ADVANCED_FACE('',(#1299),#704,.T.);
#10642=ADVANCED_FACE('',(#1300),#705,.T.);
#10643=ADVANCED_FACE('',(#1301),#706,.T.);
#10644=ADVANCED_FACE('',(#1302),#707,.T.);
#10645=ADVANCED_FACE('',(#1303),#708,.T.);
#10646=ADVANCED_FACE('',(#1304),#709,.T.);
#10647=ADVANCED_FACE('',(#1305),#710,.T.);
#10648=ADVANCED_FACE('',(#1306),#711,.T.);
#10649=ADVANCED_FACE('',(#1307),#712,.T.);
#10650=ADVANCED_FACE('',(#1308),#713,.T.);
#10651=ADVANCED_FACE('',(#1309),#714,.T.);
#10652=ADVANCED_FACE('',(#1310),#715,.T.);
#10653=ADVANCED_FACE('',(#1311),#716,.T.);
#10654=ADVANCED_FACE('',(#1312),#717,.T.);
#10655=ADVANCED_FACE('',(#1313),#718,.T.);
#10656=ADVANCED_FACE('',(#1314),#719,.T.);
#10657=ADVANCED_FACE('',(#1315),#720,.T.);
#10658=ADVANCED_FACE('',(#1316,#507),#721,.T.);
#10659=ADVANCED_FACE('',(#1317),#722,.T.);
#10660=ADVANCED_FACE('',(#1318),#723,.T.);
#10661=ADVANCED_FACE('',(#1319),#724,.T.);
#10662=ADVANCED_FACE('',(#1320),#725,.T.);
#10663=ADVANCED_FACE('',(#1321),#726,.T.);
#10664=ADVANCED_FACE('',(#1322),#727,.T.);
#10665=ADVANCED_FACE('',(#1323),#728,.T.);
#10666=ADVANCED_FACE('',(#1324),#729,.T.);
#10667=ADVANCED_FACE('',(#1325),#730,.T.);
#10668=ADVANCED_FACE('',(#1326),#731,.T.);
#10669=ADVANCED_FACE('',(#1327),#732,.T.);
#10670=ADVANCED_FACE('',(#1328),#733,.T.);
#10671=ADVANCED_FACE('',(#1329),#734,.T.);
#10672=ADVANCED_FACE('',(#1330),#735,.T.);
#10673=ADVANCED_FACE('',(#1331),#736,.T.);
#10674=ADVANCED_FACE('',(#1332),#737,.T.);
#10675=ADVANCED_FACE('',(#1333),#738,.T.);
#10676=ADVANCED_FACE('',(#1334),#739,.T.);
#10677=ADVANCED_FACE('',(#1335),#740,.T.);
#10678=ADVANCED_FACE('',(#1336),#741,.T.);
#10679=ADVANCED_FACE('',(#1337),#742,.T.);
#10680=ADVANCED_FACE('',(#1338),#743,.T.);
#10681=ADVANCED_FACE('',(#1339),#744,.T.);
#10682=ADVANCED_FACE('',(#1340),#745,.T.);
#10683=ADVANCED_FACE('',(#1341),#746,.T.);
#10684=ADVANCED_FACE('',(#1342),#747,.T.);
#10685=ADVANCED_FACE('',(#1343),#748,.T.);
#10686=ADVANCED_FACE('',(#1344),#749,.T.);
#10687=ADVANCED_FACE('',(#1345),#750,.T.);
#10688=ADVANCED_FACE('',(#1346),#751,.T.);
#10689=ADVANCED_FACE('',(#1347),#752,.T.);
#10690=ADVANCED_FACE('',(#1348),#753,.T.);
#10691=ADVANCED_FACE('',(#1349),#754,.T.);
#10692=ADVANCED_FACE('',(#1350),#755,.T.);
#10693=ADVANCED_FACE('',(#1351),#756,.T.);
#10694=ADVANCED_FACE('',(#1352),#757,.T.);
#10695=ADVANCED_FACE('',(#1353),#758,.T.);
#10696=ADVANCED_FACE('',(#1354),#759,.T.);
#10697=ADVANCED_FACE('',(#1355),#760,.T.);
#10698=ADVANCED_FACE('',(#1356),#761,.T.);
#10699=ADVANCED_FACE('',(#1357),#762,.T.);
#10700=ADVANCED_FACE('',(#1358),#763,.T.);
#10701=ADVANCED_FACE('',(#1359),#764,.T.);
#10702=ADVANCED_FACE('',(#1360),#765,.T.);
#10703=ADVANCED_FACE('',(#1361),#766,.T.);
#10704=ADVANCED_FACE('',(#1362),#767,.T.);
#10705=ADVANCED_FACE('',(#1363),#768,.T.);
#10706=ADVANCED_FACE('',(#1364),#769,.T.);
#10707=ADVANCED_FACE('',(#1365),#770,.T.);
#10708=ADVANCED_FACE('',(#1366),#771,.T.);
#10709=ADVANCED_FACE('',(#1367),#772,.T.);
#10710=ADVANCED_FACE('',(#1368),#773,.T.);
#10711=ADVANCED_FACE('',(#1369),#774,.T.);
#10712=ADVANCED_FACE('',(#1370),#775,.T.);
#10713=ADVANCED_FACE('',(#1371,#508),#10349,.T.);
#10714=ADVANCED_FACE('',(#1372,#509),#776,.F.);
#10715=ADVANCED_FACE('',(#1373),#10350,.F.);
#10716=ADVANCED_FACE('',(#1374,#510),#10351,.F.);
#10717=ADVANCED_FACE('',(#1375),#777,.T.);
#10718=ADVANCED_FACE('',(#1376),#778,.T.);
#10719=ADVANCED_FACE('',(#1377),#779,.T.);
#10720=ADVANCED_FACE('',(#1378),#780,.T.);
#10721=ADVANCED_FACE('',(#1379),#781,.T.);
#10722=ADVANCED_FACE('',(#1380),#782,.T.);
#10723=ADVANCED_FACE('',(#1381),#783,.T.);
#10724=ADVANCED_FACE('',(#1382),#784,.T.);
#10725=ADVANCED_FACE('',(#1383),#785,.T.);
#10726=ADVANCED_FACE('',(#1384),#786,.T.);
#10727=ADVANCED_FACE('',(#1385),#787,.T.);
#10728=ADVANCED_FACE('',(#1386),#788,.T.);
#10729=ADVANCED_FACE('',(#1387),#789,.T.);
#10730=ADVANCED_FACE('',(#1388),#790,.T.);
#10731=ADVANCED_FACE('',(#1389),#791,.T.);
#10732=ADVANCED_FACE('',(#1390),#792,.T.);
#10733=ADVANCED_FACE('',(#1391),#793,.T.);
#10734=ADVANCED_FACE('',(#1392),#794,.T.);
#10735=ADVANCED_FACE('',(#1393),#795,.F.);
#10736=ADVANCED_FACE('',(#1394),#796,.F.);
#10737=ADVANCED_FACE('',(#1395),#797,.F.);
#10738=ADVANCED_FACE('',(#1396),#798,.F.);
#10739=ADVANCED_FACE('',(#1397),#799,.F.);
#10740=ADVANCED_FACE('',(#1398),#800,.F.);
#10741=ADVANCED_FACE('',(#1399),#801,.F.);
#10742=ADVANCED_FACE('',(#1400,#511),#802,.F.);
#10743=ADVANCED_FACE('',(#1401),#803,.F.);
#10744=ADVANCED_FACE('',(#1402),#804,.F.);
#10745=ADVANCED_FACE('',(#1403),#805,.T.);
#10746=ADVANCED_FACE('',(#1404),#806,.T.);
#10747=ADVANCED_FACE('',(#1405),#807,.T.);
#10748=ADVANCED_FACE('',(#1406),#808,.T.);
#10749=ADVANCED_FACE('',(#1407),#809,.T.);
#10750=ADVANCED_FACE('',(#1408),#810,.T.);
#10751=ADVANCED_FACE('',(#1409),#811,.T.);
#10752=ADVANCED_FACE('',(#1410),#812,.T.);
#10753=ADVANCED_FACE('',(#1411),#813,.T.);
#10754=ADVANCED_FACE('',(#1412),#814,.T.);
#10755=ADVANCED_FACE('',(#1413),#815,.T.);
#10756=ADVANCED_FACE('',(#1414),#816,.T.);
#10757=ADVANCED_FACE('',(#1415),#817,.T.);
#10758=ADVANCED_FACE('',(#1416),#818,.T.);
#10759=ADVANCED_FACE('',(#1417),#819,.T.);
#10760=ADVANCED_FACE('',(#1418),#820,.T.);
#10761=ADVANCED_FACE('',(#1419),#821,.T.);
#10762=ADVANCED_FACE('',(#1420),#822,.T.);
#10763=ADVANCED_FACE('',(#1421),#823,.F.);
#10764=ADVANCED_FACE('',(#1422),#824,.F.);
#10765=ADVANCED_FACE('',(#1423),#825,.F.);
#10766=ADVANCED_FACE('',(#1424),#826,.F.);
#10767=ADVANCED_FACE('',(#1425),#827,.F.);
#10768=ADVANCED_FACE('',(#1426),#828,.F.);
#10769=ADVANCED_FACE('',(#1427),#829,.F.);
#10770=ADVANCED_FACE('',(#1428),#830,.F.);
#10771=ADVANCED_FACE('',(#1429),#831,.F.);
#10772=ADVANCED_FACE('',(#1430),#832,.T.);
#10773=ADVANCED_FACE('',(#1431),#833,.T.);
#10774=ADVANCED_FACE('',(#1432),#834,.T.);
#10775=ADVANCED_FACE('',(#1433),#835,.T.);
#10776=ADVANCED_FACE('',(#1434),#836,.T.);
#10777=ADVANCED_FACE('',(#1435),#837,.T.);
#10778=ADVANCED_FACE('',(#1436),#838,.T.);
#10779=ADVANCED_FACE('',(#1437),#839,.T.);
#10780=ADVANCED_FACE('',(#1438),#840,.T.);
#10781=ADVANCED_FACE('',(#1439),#841,.T.);
#10782=ADVANCED_FACE('',(#1440),#842,.T.);
#10783=ADVANCED_FACE('',(#1441),#843,.T.);
#10784=ADVANCED_FACE('',(#1442),#844,.T.);
#10785=ADVANCED_FACE('',(#1443),#845,.T.);
#10786=ADVANCED_FACE('',(#1444),#846,.T.);
#10787=ADVANCED_FACE('',(#1445),#847,.T.);
#10788=ADVANCED_FACE('',(#1446),#848,.T.);
#10789=ADVANCED_FACE('',(#1447),#849,.T.);
#10790=ADVANCED_FACE('',(#1448),#850,.F.);
#10791=ADVANCED_FACE('',(#1449),#851,.F.);
#10792=ADVANCED_FACE('',(#1450),#852,.F.);
#10793=ADVANCED_FACE('',(#1451),#853,.F.);
#10794=ADVANCED_FACE('',(#1452),#854,.F.);
#10795=ADVANCED_FACE('',(#1453),#855,.F.);
#10796=ADVANCED_FACE('',(#1454),#856,.F.);
#10797=ADVANCED_FACE('',(#1455),#857,.F.);
#10798=ADVANCED_FACE('',(#1456),#858,.F.);
#10799=ADVANCED_FACE('',(#1457,#512),#10352,.T.);
#10800=ADVANCED_FACE('',(#1458,#513),#859,.T.);
#10801=ADVANCED_FACE('',(#1459),#860,.F.);
#10802=ADVANCED_FACE('',(#1460),#10353,.T.);
#10803=ADVANCED_FACE('',(#1461),#10354,.T.);
#10804=ADVANCED_FACE('',(#1462),#10355,.T.);
#10805=ADVANCED_FACE('',(#1463),#10356,.T.);
#10806=ADVANCED_FACE('',(#1464),#10357,.T.);
#10807=ADVANCED_FACE('',(#1465),#10358,.T.);
#10808=ADVANCED_FACE('',(#1466),#861,.T.);
#10809=ADVANCED_FACE('',(#1467),#862,.T.);
#10810=ADVANCED_FACE('',(#1468),#863,.T.);
#10811=ADVANCED_FACE('',(#1469),#864,.T.);
#10812=ADVANCED_FACE('',(#1470),#865,.T.);
#10813=ADVANCED_FACE('',(#1471),#866,.T.);
#10814=ADVANCED_FACE('',(#1472),#867,.T.);
#10815=ADVANCED_FACE('',(#1473),#868,.T.);
#10816=ADVANCED_FACE('',(#1474),#869,.T.);
#10817=ADVANCED_FACE('',(#1475),#870,.T.);
#10818=ADVANCED_FACE('',(#1476),#871,.T.);
#10819=ADVANCED_FACE('',(#1477),#872,.T.);
#10820=ADVANCED_FACE('',(#1478),#873,.T.);
#10821=ADVANCED_FACE('',(#1479),#874,.T.);
#10822=ADVANCED_FACE('',(#1480),#875,.T.);
#10823=ADVANCED_FACE('',(#1481),#876,.T.);
#10824=ADVANCED_FACE('',(#1482),#877,.T.);
#10825=ADVANCED_FACE('',(#1483),#878,.T.);
#10826=ADVANCED_FACE('',(#1484),#879,.T.);
#10827=ADVANCED_FACE('',(#1485),#880,.T.);
#10828=ADVANCED_FACE('',(#1486),#881,.T.);
#10829=ADVANCED_FACE('',(#1487),#882,.T.);
#10830=ADVANCED_FACE('',(#1488),#883,.T.);
#10831=ADVANCED_FACE('',(#1489),#884,.T.);
#10832=ADVANCED_FACE('',(#1490),#885,.T.);
#10833=ADVANCED_FACE('',(#1491),#886,.T.);
#10834=ADVANCED_FACE('',(#1492),#887,.T.);
#10835=ADVANCED_FACE('',(#1493),#888,.T.);
#10836=ADVANCED_FACE('',(#1494),#889,.T.);
#10837=ADVANCED_FACE('',(#1495),#890,.T.);
#10838=ADVANCED_FACE('',(#1496),#891,.T.);
#10839=ADVANCED_FACE('',(#1497),#892,.T.);
#10840=ADVANCED_FACE('',(#1498),#893,.T.);
#10841=ADVANCED_FACE('',(#1499),#894,.T.);
#10842=ADVANCED_FACE('',(#1500),#895,.T.);
#10843=ADVANCED_FACE('',(#1501),#896,.T.);
#10844=ADVANCED_FACE('',(#1502),#897,.T.);
#10845=ADVANCED_FACE('',(#1503),#898,.T.);
#10846=ADVANCED_FACE('',(#1504),#899,.T.);
#10847=ADVANCED_FACE('',(#1505),#900,.T.);
#10848=ADVANCED_FACE('',(#1506),#901,.T.);
#10849=ADVANCED_FACE('',(#1507),#902,.T.);
#10850=ADVANCED_FACE('',(#1508),#903,.T.);
#10851=ADVANCED_FACE('',(#1509),#904,.T.);
#10852=ADVANCED_FACE('',(#1510),#905,.T.);
#10853=ADVANCED_FACE('',(#1511),#906,.T.);
#10854=ADVANCED_FACE('',(#1512),#907,.T.);
#10855=ADVANCED_FACE('',(#1513),#908,.T.);
#10856=ADVANCED_FACE('',(#1514),#909,.T.);
#10857=ADVANCED_FACE('',(#1515),#910,.T.);
#10858=ADVANCED_FACE('',(#1516),#911,.T.);
#10859=ADVANCED_FACE('',(#1517),#912,.T.);
#10860=ADVANCED_FACE('',(#1518),#913,.T.);
#10861=ADVANCED_FACE('',(#1519),#914,.T.);
#10862=ADVANCED_FACE('',(#1520),#915,.T.);
#10863=ADVANCED_FACE('',(#1521),#916,.T.);
#10864=ADVANCED_FACE('',(#1522),#917,.T.);
#10865=ADVANCED_FACE('',(#1523),#918,.T.);
#10866=ADVANCED_FACE('',(#1524),#919,.T.);
#10867=ADVANCED_FACE('',(#1525),#920,.T.);
#10868=ADVANCED_FACE('',(#1526),#921,.T.);
#10869=ADVANCED_FACE('',(#1527),#922,.T.);
#10870=ADVANCED_FACE('',(#1528),#923,.T.);
#10871=ADVANCED_FACE('',(#1529),#924,.T.);
#10872=ADVANCED_FACE('',(#1530),#925,.T.);
#10873=ADVANCED_FACE('',(#1531),#926,.T.);
#10874=ADVANCED_FACE('',(#1532),#927,.T.);
#10875=ADVANCED_FACE('',(#1533),#928,.T.);
#10876=ADVANCED_FACE('',(#1534),#929,.T.);
#10877=ADVANCED_FACE('',(#1535),#930,.T.);
#10878=ADVANCED_FACE('',(#1536),#931,.T.);
#10879=ADVANCED_FACE('',(#1537),#932,.T.);
#10880=ADVANCED_FACE('',(#1538),#933,.T.);
#10881=ADVANCED_FACE('',(#1539),#934,.T.);
#10882=ADVANCED_FACE('',(#1540),#935,.T.);
#10883=ADVANCED_FACE('',(#1541),#936,.T.);
#10884=ADVANCED_FACE('',(#1542),#937,.T.);
#10885=ADVANCED_FACE('',(#1543),#938,.T.);
#10886=ADVANCED_FACE('',(#1544),#939,.T.);
#10887=ADVANCED_FACE('',(#1545),#940,.T.);
#10888=ADVANCED_FACE('',(#1546),#941,.T.);
#10889=ADVANCED_FACE('',(#1547),#942,.T.);
#10890=ADVANCED_FACE('',(#1548),#943,.T.);
#10891=ADVANCED_FACE('',(#1549),#944,.T.);
#10892=ADVANCED_FACE('',(#1550),#945,.T.);
#10893=ADVANCED_FACE('',(#1551),#946,.T.);
#10894=ADVANCED_FACE('',(#1552),#947,.T.);
#10895=ADVANCED_FACE('',(#1553),#948,.T.);
#10896=ADVANCED_FACE('',(#1554),#949,.T.);
#10897=ADVANCED_FACE('',(#1555),#950,.T.);
#10898=ADVANCED_FACE('',(#1556),#951,.T.);
#10899=ADVANCED_FACE('',(#1557),#952,.T.);
#10900=ADVANCED_FACE('',(#1558),#953,.T.);
#10901=ADVANCED_FACE('',(#1559),#954,.T.);
#10902=ADVANCED_FACE('',(#1560),#955,.T.);
#10903=ADVANCED_FACE('',(#1561),#956,.T.);
#10904=ADVANCED_FACE('',(#1562),#957,.T.);
#10905=ADVANCED_FACE('',(#1563),#958,.T.);
#10906=ADVANCED_FACE('',(#1564),#959,.T.);
#10907=ADVANCED_FACE('',(#1565),#960,.T.);
#10908=ADVANCED_FACE('',(#1566),#961,.T.);
#10909=ADVANCED_FACE('',(#1567),#962,.T.);
#10910=ADVANCED_FACE('',(#1568),#963,.T.);
#10911=ADVANCED_FACE('',(#1569),#964,.T.);
#10912=ADVANCED_FACE('',(#1570),#965,.T.);
#10913=ADVANCED_FACE('',(#1571),#966,.T.);
#10914=ADVANCED_FACE('',(#1572),#967,.T.);
#10915=ADVANCED_FACE('',(#1573),#968,.T.);
#10916=ADVANCED_FACE('',(#1574),#969,.T.);
#10917=ADVANCED_FACE('',(#1575),#970,.T.);
#10918=ADVANCED_FACE('',(#1576),#971,.T.);
#10919=ADVANCED_FACE('',(#1577),#972,.T.);
#10920=ADVANCED_FACE('',(#1578),#973,.T.);
#10921=ADVANCED_FACE('',(#1579),#974,.T.);
#10922=ADVANCED_FACE('',(#1580),#975,.T.);
#10923=ADVANCED_FACE('',(#1581),#976,.T.);
#10924=ADVANCED_FACE('',(#1582),#977,.T.);
#10925=ADVANCED_FACE('',(#1583),#978,.T.);
#10926=ADVANCED_FACE('',(#1584),#979,.T.);
#10927=ADVANCED_FACE('',(#1585),#980,.T.);
#10928=ADVANCED_FACE('',(#1586),#981,.T.);
#10929=ADVANCED_FACE('',(#1587),#982,.T.);
#10930=ADVANCED_FACE('',(#1588),#983,.T.);
#10931=ADVANCED_FACE('',(#1589),#984,.T.);
#10932=ADVANCED_FACE('',(#1590),#985,.T.);
#10933=ADVANCED_FACE('',(#1591),#986,.T.);
#10934=ADVANCED_FACE('',(#1592),#987,.T.);
#10935=ADVANCED_FACE('',(#1593),#988,.T.);
#10936=ADVANCED_FACE('',(#1594),#989,.T.);
#10937=ADVANCED_FACE('',(#1595),#990,.T.);
#10938=ADVANCED_FACE('',(#1596),#991,.T.);
#10939=ADVANCED_FACE('',(#1597),#992,.T.);
#10940=ADVANCED_FACE('',(#1598),#993,.T.);
#10941=ADVANCED_FACE('',(#1599),#994,.T.);
#10942=ADVANCED_FACE('',(#1600),#19,.T.);
#10943=ADVANCED_FACE('',(#1601),#995,.T.);
#10944=ADVANCED_FACE('',(#1602),#20,.T.);
#10945=ADVANCED_FACE('',(#1603),#10359,.T.);
#10946=ADVANCED_FACE('',(#1604),#996,.T.);
#10947=ADVANCED_FACE('',(#1605),#997,.T.);
#10948=ADVANCED_FACE('',(#1606),#998,.T.);
#10949=ADVANCED_FACE('',(#1607),#21,.T.);
#10950=ADVANCED_FACE('',(#1608),#999,.T.);
#10951=ADVANCED_FACE('',(#1609),#22,.T.);
#10952=ADVANCED_FACE('',(#1610),#10360,.T.);
#10953=ADVANCED_FACE('',(#1611),#1000,.F.);
#10954=ADVANCED_FACE('',(#1612),#1001,.T.);
#10955=ADVANCED_FACE('',(#1613),#1002,.F.);
#10956=ADVANCED_FACE('',(#1614),#1003,.F.);
#10957=ADVANCED_FACE('',(#1615),#1004,.F.);
#10958=ADVANCED_FACE('',(#1616),#1005,.F.);
#10959=ADVANCED_FACE('',(#1617),#1006,.F.);
#10960=ADVANCED_FACE('',(#1618),#1007,.F.);
#10961=ADVANCED_FACE('',(#1619),#1008,.F.);
#10962=ADVANCED_FACE('',(#1620,#514),#1009,.T.);
#10963=ADVANCED_FACE('',(#1621),#23,.T.);
#10964=ADVANCED_FACE('',(#1622),#10361,.T.);
#10965=ADVANCED_FACE('',(#1623),#24,.T.);
#10966=ADVANCED_FACE('',(#1624),#1010,.T.);
#10967=ADVANCED_FACE('',(#1625),#1011,.T.);
#10968=ADVANCED_FACE('',(#1626),#25,.T.);
#10969=ADVANCED_FACE('',(#1627),#10362,.T.);
#10970=ADVANCED_FACE('',(#1628),#26,.T.);
#10971=ADVANCED_FACE('',(#1629,#515),#1012,.T.);
#10972=ADVANCED_FACE('',(#1630),#27,.T.);
#10973=ADVANCED_FACE('',(#1631),#10363,.T.);
#10974=ADVANCED_FACE('',(#1632),#28,.T.);
#10975=ADVANCED_FACE('',(#1633),#1013,.T.);
#10976=ADVANCED_FACE('',(#1634),#1014,.F.);
#10977=ADVANCED_FACE('',(#1635),#1015,.F.);
#10978=ADVANCED_FACE('',(#1636),#1016,.F.);
#10979=ADVANCED_FACE('',(#1637),#1017,.F.);
#10980=ADVANCED_FACE('',(#1638),#1018,.F.);
#10981=ADVANCED_FACE('',(#1639),#1019,.F.);
#10982=ADVANCED_FACE('',(#1640),#1020,.F.);
#10983=ADVANCED_FACE('',(#1641),#1021,.F.);
#10984=CLOSED_SHELL('',(#10364,#10365,#10366,#10367,#10368,#10369,#10370,
#10371,#10372,#10373,#10374,#10375));
#10985=CLOSED_SHELL('',(#10376,#10377,#10378,#10379,#10380,#10381));
#10986=CLOSED_SHELL('',(#10382,#10383,#10384,#10385,#10386,#10387));
#10987=CLOSED_SHELL('',(#10388,#10389,#10390,#10391));
#10988=CLOSED_SHELL('',(#10392,#10393,#10394,#10395));
#10989=CLOSED_SHELL('',(#10396,#10397,#10398,#10399));
#10990=CLOSED_SHELL('',(#10400,#10401,#10402,#10403));
#10991=CLOSED_SHELL('',(#10404,#10405,#10406,#10407,#10408,#10409,#10410,
#10411,#10412,#10413,#10414,#10415,#10416,#10417,#10418));
#10992=CLOSED_SHELL('',(#10419,#10420,#10421,#10422,#10423,#10424,#10425,
#10426,#10427,#10428,#10429,#10430,#10431,#10432,#10433,#10434,#10435));
#10993=CLOSED_SHELL('',(#10436,#10437,#10438,#10439,#10440,#10441,#10442,
#10443,#10444,#10445,#10446,#10447));
#10994=CLOSED_SHELL('',(#10448,#10449,#10450,#10451,#10452,#10453,#10454,
#10455,#10456,#10457,#10458,#10459));
#10995=CLOSED_SHELL('',(#10460,#10461,#10462,#10463,#10464,#10465,#10466,
#10467,#10468,#10469,#10470,#10471));
#10996=CLOSED_SHELL('',(#10472,#10473,#10474,#10475,#10476,#10477,#10478,
#10479,#10480,#10481,#10482,#10483));
#10997=CLOSED_SHELL('',(#10484,#10485,#10486,#10487,#10488,#10489,#10490,
#10491,#10492,#10493,#10494,#10495,#10496,#10497,#10498,#10499,#10500,#10501,
#10502,#10503,#10504,#10505,#10506,#10507,#10508,#10509,#10510,#10511,#10512));
#10998=CLOSED_SHELL('',(#10513,#10514,#10515,#10516));
#10999=CLOSED_SHELL('',(#10517,#10518,#10519,#10520,#10521,#10522,#10523,
#10524,#10525,#10526,#10527,#10528));
#11000=CLOSED_SHELL('',(#10529,#10530,#10531,#10532));
#11001=CLOSED_SHELL('',(#10533,#10534,#10535,#10536,#10537,#10538,#10539,
#10540));
#11002=CLOSED_SHELL('',(#10541,#10542,#10543,#10544,#10545,#10546,#10547,
#10548));
#11003=CLOSED_SHELL('',(#10549,#10550,#10551,#10552,#10553,#10554,#10555,
#10556));
#11004=CLOSED_SHELL('',(#10557,#10558,#10559,#10560,#10561,#10562,#10563,
#10564));
#11005=CLOSED_SHELL('',(#10565,#10566,#10567,#10568,#10569,#10570,#10571,
#10572,#10573,#10574));
#11006=CLOSED_SHELL('',(#10575,#10576,#10577));
#11007=CLOSED_SHELL('',(#10578,#10579,#10580,#10581,#10582,#10583,#10584));
#11008=CLOSED_SHELL('',(#10585,#10586,#10587,#10588,#10589,#10590,#10591,
#10592,#10593,#10594,#10595,#10596,#10597,#10598));
#11009=CLOSED_SHELL('',(#10599,#10600,#10601,#10602,#10603,#10604,#10605));
#11010=CLOSED_SHELL('',(#10606,#10607,#10608,#10609,#10610,#10611,#10612));
#11011=CLOSED_SHELL('',(#10613,#10614,#10615,#10616));
#11012=CLOSED_SHELL('',(#10617,#10618,#10619,#10620,#10621,#10622,#10623,
#10624,#10625,#10626,#10627,#10628));
#11013=CLOSED_SHELL('',(#10629,#10630,#10631,#10632,#10633,#10634,#10635,
#10636,#10637,#10638,#10639,#10640,#10641,#10642,#10643,#10644,#10645,#10646,
#10647,#10648,#10649,#10650,#10651,#10652,#10653,#10654,#10655,#10656,#10657,
#10658,#10659,#10660,#10661,#10662,#10663,#10664,#10665,#10666,#10667,#10668,
#10669,#10670,#10671,#10672,#10673,#10674,#10675,#10676,#10677,#10678,#10679,
#10680,#10681,#10682,#10683,#10684,#10685,#10686,#10687,#10688,#10689,#10690,
#10691,#10692,#10693,#10694,#10695,#10696,#10697,#10698,#10699,#10700,#10701,
#10702,#10703,#10704,#10705,#10706,#10707,#10708,#10709,#10710,#10711,#10712,
#10713,#10714));
#11014=CLOSED_SHELL('',(#10715,#10716,#10717,#10718,#10719,#10720,#10721,
#10722,#10723,#10724,#10725,#10726,#10727,#10728,#10729,#10730,#10731,#10732,
#10733,#10734,#10735,#10736,#10737,#10738,#10739,#10740,#10741,#10742,#10743,
#10744,#10745,#10746,#10747,#10748,#10749,#10750,#10751,#10752,#10753,#10754,
#10755,#10756,#10757,#10758,#10759,#10760,#10761,#10762,#10763,#10764,#10765,
#10766,#10767,#10768,#10769,#10770,#10771,#10772,#10773,#10774,#10775,#10776,
#10777,#10778,#10779,#10780,#10781,#10782,#10783,#10784,#10785,#10786,#10787,
#10788,#10789,#10790,#10791,#10792,#10793,#10794,#10795,#10796,#10797,#10798,
#10799,#10800));
#11015=CLOSED_SHELL('',(#10801,#10802,#10803,#10804,#10805,#10806,#10807,
#10808,#10809,#10810,#10811,#10812,#10813,#10814,#10815,#10816,#10817,#10818,
#10819,#10820,#10821,#10822,#10823,#10824,#10825,#10826,#10827,#10828,#10829,
#10830,#10831,#10832,#10833,#10834,#10835,#10836,#10837,#10838,#10839,#10840,
#10841,#10842,#10843,#10844,#10845,#10846,#10847,#10848,#10849,#10850,#10851,
#10852,#10853,#10854,#10855,#10856,#10857,#10858,#10859,#10860,#10861,#10862,
#10863,#10864,#10865,#10866,#10867,#10868,#10869,#10870,#10871,#10872,#10873,
#10874,#10875,#10876,#10877,#10878,#10879,#10880,#10881,#10882,#10883,#10884,
#10885,#10886,#10887,#10888,#10889,#10890,#10891,#10892,#10893,#10894,#10895,
#10896,#10897,#10898,#10899,#10900,#10901,#10902,#10903,#10904,#10905,#10906,
#10907,#10908,#10909,#10910,#10911,#10912,#10913,#10914,#10915,#10916,#10917,
#10918,#10919,#10920,#10921,#10922,#10923,#10924,#10925,#10926,#10927,#10928,
#10929,#10930,#10931,#10932,#10933,#10934,#10935,#10936,#10937,#10938,#10939,
#10940));
#11016=CLOSED_SHELL('',(#10941,#10942,#10943,#10944,#10945,#10946,#10947,
#10948,#10949,#10950,#10951,#10952,#10953,#10954));
#11017=CLOSED_SHELL('',(#10955,#10956,#10957,#10958,#10959,#10960,#10961,
#10962,#10963,#10964,#10965,#10966));
#11018=CLOSED_SHELL('',(#10967,#10968,#10969,#10970,#10971,#10972,#10973,
#10974,#10975));
#11019=CLOSED_SHELL('',(#10976,#10977,#10978,#10979,#10980,#10981,#10982,
#10983));
#11020=DERIVED_UNIT_ELEMENT(#11084,1.);
#11021=DERIVED_UNIT_ELEMENT(#19363,-3.);
#11022=DERIVED_UNIT_ELEMENT(#11084,1.);
#11023=DERIVED_UNIT_ELEMENT(#19363,-3.);
#11024=DERIVED_UNIT_ELEMENT(#11084,1.);
#11025=DERIVED_UNIT_ELEMENT(#19363,-3.);
#11026=DERIVED_UNIT_ELEMENT(#11084,1.);
#11027=DERIVED_UNIT_ELEMENT(#19363,-3.);
#11028=DERIVED_UNIT_ELEMENT(#11084,1.);
#11029=DERIVED_UNIT_ELEMENT(#19363,-3.);
#11030=DERIVED_UNIT_ELEMENT(#11084,1.);
#11031=DERIVED_UNIT_ELEMENT(#19363,-3.);
#11032=DERIVED_UNIT_ELEMENT(#11084,1.);
#11033=DERIVED_UNIT_ELEMENT(#19363,-3.);
#11034=DERIVED_UNIT_ELEMENT(#11084,1.);
#11035=DERIVED_UNIT_ELEMENT(#19363,-3.);
#11036=DERIVED_UNIT_ELEMENT(#11084,1.);
#11037=DERIVED_UNIT_ELEMENT(#19363,-3.);
#11038=DERIVED_UNIT_ELEMENT(#11084,1.);
#11039=DERIVED_UNIT_ELEMENT(#19363,-3.);
#11040=DERIVED_UNIT_ELEMENT(#11084,1.);
#11041=DERIVED_UNIT_ELEMENT(#19363,-3.);
#11042=DERIVED_UNIT_ELEMENT(#11084,1.);
#11043=DERIVED_UNIT_ELEMENT(#19363,-3.);
#11044=DERIVED_UNIT_ELEMENT(#11084,1.);
#11045=DERIVED_UNIT_ELEMENT(#19363,-3.);
#11046=DERIVED_UNIT_ELEMENT(#11084,1.);
#11047=DERIVED_UNIT_ELEMENT(#19363,-3.);
#11048=DERIVED_UNIT_ELEMENT(#11084,1.);
#11049=DERIVED_UNIT_ELEMENT(#19363,-3.);
#11050=DERIVED_UNIT_ELEMENT(#11084,1.);
#11051=DERIVED_UNIT_ELEMENT(#19363,-3.);
#11052=DERIVED_UNIT_ELEMENT(#11084,1.);
#11053=DERIVED_UNIT_ELEMENT(#19363,-3.);
#11054=DERIVED_UNIT_ELEMENT(#11084,1.);
#11055=DERIVED_UNIT_ELEMENT(#19363,-3.);
#11056=DERIVED_UNIT_ELEMENT(#11084,1.);
#11057=DERIVED_UNIT_ELEMENT(#19363,-3.);
#11058=DERIVED_UNIT_ELEMENT(#11084,1.);
#11059=DERIVED_UNIT_ELEMENT(#19363,-3.);
#11060=DERIVED_UNIT_ELEMENT(#11084,1.);
#11061=DERIVED_UNIT_ELEMENT(#19363,-3.);
#11062=DERIVED_UNIT_ELEMENT(#11084,1.);
#11063=DERIVED_UNIT_ELEMENT(#19363,-3.);
#11064=DERIVED_UNIT_ELEMENT(#11084,1.);
#11065=DERIVED_UNIT_ELEMENT(#19363,-3.);
#11066=DERIVED_UNIT_ELEMENT(#11084,1.);
#11067=DERIVED_UNIT_ELEMENT(#19363,-3.);
#11068=DERIVED_UNIT_ELEMENT(#11084,1.);
#11069=DERIVED_UNIT_ELEMENT(#19363,-3.);
#11070=DERIVED_UNIT_ELEMENT(#11084,1.);
#11071=DERIVED_UNIT_ELEMENT(#19363,-3.);
#11072=DERIVED_UNIT_ELEMENT(#11084,1.);
#11073=DERIVED_UNIT_ELEMENT(#19363,-3.);
#11074=DERIVED_UNIT_ELEMENT(#11084,1.);
#11075=DERIVED_UNIT_ELEMENT(#19363,-3.);
#11076=DERIVED_UNIT_ELEMENT(#11084,1.);
#11077=DERIVED_UNIT_ELEMENT(#19363,-3.);
#11078=DERIVED_UNIT_ELEMENT(#11084,1.);
#11079=DERIVED_UNIT_ELEMENT(#19363,-3.);
#11080=DERIVED_UNIT_ELEMENT(#11084,1.);
#11081=DERIVED_UNIT_ELEMENT(#19363,-3.);
#11082=DERIVED_UNIT_ELEMENT(#11084,1.);
#11083=DERIVED_UNIT_ELEMENT(#19363,-3.);
#11084=(
MASS_UNIT()
NAMED_UNIT(*)
SI_UNIT(.KILO.,.GRAM.)
);
#11085=DERIVED_UNIT((#11020,#11021));
#11086=DERIVED_UNIT((#11022,#11023));
#11087=DERIVED_UNIT((#11024,#11025));
#11088=DERIVED_UNIT((#11026,#11027));
#11089=DERIVED_UNIT((#11028,#11029));
#11090=DERIVED_UNIT((#11030,#11031));
#11091=DERIVED_UNIT((#11032,#11033));
#11092=DERIVED_UNIT((#11034,#11035));
#11093=DERIVED_UNIT((#11036,#11037));
#11094=DERIVED_UNIT((#11038,#11039));
#11095=DERIVED_UNIT((#11040,#11041));
#11096=DERIVED_UNIT((#11042,#11043));
#11097=DERIVED_UNIT((#11044,#11045));
#11098=DERIVED_UNIT((#11046,#11047));
#11099=DERIVED_UNIT((#11048,#11049));
#11100=DERIVED_UNIT((#11050,#11051));
#11101=DERIVED_UNIT((#11052,#11053));
#11102=DERIVED_UNIT((#11054,#11055));
#11103=DERIVED_UNIT((#11056,#11057));
#11104=DERIVED_UNIT((#11058,#11059));
#11105=DERIVED_UNIT((#11060,#11061));
#11106=DERIVED_UNIT((#11062,#11063));
#11107=DERIVED_UNIT((#11064,#11065));
#11108=DERIVED_UNIT((#11066,#11067));
#11109=DERIVED_UNIT((#11068,#11069));
#11110=DERIVED_UNIT((#11070,#11071));
#11111=DERIVED_UNIT((#11072,#11073));
#11112=DERIVED_UNIT((#11074,#11075));
#11113=DERIVED_UNIT((#11076,#11077));
#11114=DERIVED_UNIT((#11078,#11079));
#11115=DERIVED_UNIT((#11080,#11081));
#11116=DERIVED_UNIT((#11082,#11083));
#11117=MEASURE_REPRESENTATION_ITEM('density measure',
POSITIVE_RATIO_MEASURE(7850.),#11085);
#11118=MEASURE_REPRESENTATION_ITEM('density measure',
POSITIVE_RATIO_MEASURE(7850.),#11086);
#11119=MEASURE_REPRESENTATION_ITEM('density measure',
POSITIVE_RATIO_MEASURE(7850.),#11087);
#11120=MEASURE_REPRESENTATION_ITEM('density measure',
POSITIVE_RATIO_MEASURE(7850.),#11088);
#11121=MEASURE_REPRESENTATION_ITEM('density measure',
POSITIVE_RATIO_MEASURE(7850.),#11089);
#11122=MEASURE_REPRESENTATION_ITEM('density measure',
POSITIVE_RATIO_MEASURE(7850.),#11090);
#11123=MEASURE_REPRESENTATION_ITEM('density measure',
POSITIVE_RATIO_MEASURE(7850.),#11091);
#11124=MEASURE_REPRESENTATION_ITEM('density measure',
POSITIVE_RATIO_MEASURE(7850.),#11092);
#11125=MEASURE_REPRESENTATION_ITEM('density measure',
POSITIVE_RATIO_MEASURE(7850.),#11093);
#11126=MEASURE_REPRESENTATION_ITEM('density measure',
POSITIVE_RATIO_MEASURE(7850.),#11094);
#11127=MEASURE_REPRESENTATION_ITEM('density measure',
POSITIVE_RATIO_MEASURE(7850.),#11095);
#11128=MEASURE_REPRESENTATION_ITEM('density measure',
POSITIVE_RATIO_MEASURE(7850.),#11096);
#11129=MEASURE_REPRESENTATION_ITEM('density measure',
POSITIVE_RATIO_MEASURE(7850.),#11097);
#11130=MEASURE_REPRESENTATION_ITEM('density measure',
POSITIVE_RATIO_MEASURE(7850.),#11098);
#11131=MEASURE_REPRESENTATION_ITEM('density measure',
POSITIVE_RATIO_MEASURE(7850.),#11099);
#11132=MEASURE_REPRESENTATION_ITEM('density measure',
POSITIVE_RATIO_MEASURE(7850.),#11100);
#11133=MEASURE_REPRESENTATION_ITEM('density measure',
POSITIVE_RATIO_MEASURE(7850.),#11101);
#11134=MEASURE_REPRESENTATION_ITEM('density measure',
POSITIVE_RATIO_MEASURE(7850.),#11102);
#11135=MEASURE_REPRESENTATION_ITEM('density measure',
POSITIVE_RATIO_MEASURE(7850.),#11103);
#11136=MEASURE_REPRESENTATION_ITEM('density measure',
POSITIVE_RATIO_MEASURE(7850.),#11104);
#11137=MEASURE_REPRESENTATION_ITEM('density measure',
POSITIVE_RATIO_MEASURE(7850.),#11105);
#11138=MEASURE_REPRESENTATION_ITEM('density measure',
POSITIVE_RATIO_MEASURE(7850.),#11106);
#11139=MEASURE_REPRESENTATION_ITEM('density measure',
POSITIVE_RATIO_MEASURE(7850.),#11107);
#11140=MEASURE_REPRESENTATION_ITEM('density measure',
POSITIVE_RATIO_MEASURE(7850.),#11108);
#11141=MEASURE_REPRESENTATION_ITEM('density measure',
POSITIVE_RATIO_MEASURE(7850.),#11109);
#11142=MEASURE_REPRESENTATION_ITEM('density measure',
POSITIVE_RATIO_MEASURE(7850.),#11110);
#11143=MEASURE_REPRESENTATION_ITEM('density measure',
POSITIVE_RATIO_MEASURE(7850.),#11111);
#11144=MEASURE_REPRESENTATION_ITEM('density measure',
POSITIVE_RATIO_MEASURE(7850.),#11112);
#11145=MEASURE_REPRESENTATION_ITEM('density measure',
POSITIVE_RATIO_MEASURE(7850.),#11113);
#11146=MEASURE_REPRESENTATION_ITEM('density measure',
POSITIVE_RATIO_MEASURE(7850.),#11114);
#11147=MEASURE_REPRESENTATION_ITEM('density measure',
POSITIVE_RATIO_MEASURE(7850.),#11115);
#11148=MEASURE_REPRESENTATION_ITEM('density measure',
POSITIVE_RATIO_MEASURE(7850.),#11116);
#11149=PROPERTY_DEFINITION_REPRESENTATION(#11309,#11213);
#11150=PROPERTY_DEFINITION_REPRESENTATION(#11310,#11214);
#11151=PROPERTY_DEFINITION_REPRESENTATION(#11311,#11215);
#11152=PROPERTY_DEFINITION_REPRESENTATION(#11312,#11216);
#11153=PROPERTY_DEFINITION_REPRESENTATION(#11313,#11217);
#11154=PROPERTY_DEFINITION_REPRESENTATION(#11314,#11218);
#11155=PROPERTY_DEFINITION_REPRESENTATION(#11315,#11219);
#11156=PROPERTY_DEFINITION_REPRESENTATION(#11316,#11220);
#11157=PROPERTY_DEFINITION_REPRESENTATION(#11317,#11221);
#11158=PROPERTY_DEFINITION_REPRESENTATION(#11318,#11222);
#11159=PROPERTY_DEFINITION_REPRESENTATION(#11319,#11223);
#11160=PROPERTY_DEFINITION_REPRESENTATION(#11320,#11224);
#11161=PROPERTY_DEFINITION_REPRESENTATION(#11321,#11225);
#11162=PROPERTY_DEFINITION_REPRESENTATION(#11322,#11226);
#11163=PROPERTY_DEFINITION_REPRESENTATION(#11323,#11227);
#11164=PROPERTY_DEFINITION_REPRESENTATION(#11324,#11228);
#11165=PROPERTY_DEFINITION_REPRESENTATION(#11325,#11229);
#11166=PROPERTY_DEFINITION_REPRESENTATION(#11326,#11230);
#11167=PROPERTY_DEFINITION_REPRESENTATION(#11327,#11231);
#11168=PROPERTY_DEFINITION_REPRESENTATION(#11328,#11232);
#11169=PROPERTY_DEFINITION_REPRESENTATION(#11329,#11233);
#11170=PROPERTY_DEFINITION_REPRESENTATION(#11330,#11234);
#11171=PROPERTY_DEFINITION_REPRESENTATION(#11331,#11235);
#11172=PROPERTY_DEFINITION_REPRESENTATION(#11332,#11236);
#11173=PROPERTY_DEFINITION_REPRESENTATION(#11333,#11237);
#11174=PROPERTY_DEFINITION_REPRESENTATION(#11334,#11238);
#11175=PROPERTY_DEFINITION_REPRESENTATION(#11335,#11239);
#11176=PROPERTY_DEFINITION_REPRESENTATION(#11336,#11240);
#11177=PROPERTY_DEFINITION_REPRESENTATION(#11337,#11241);
#11178=PROPERTY_DEFINITION_REPRESENTATION(#11338,#11242);
#11179=PROPERTY_DEFINITION_REPRESENTATION(#11339,#11243);
#11180=PROPERTY_DEFINITION_REPRESENTATION(#11340,#11244);
#11181=PROPERTY_DEFINITION_REPRESENTATION(#11341,#11245);
#11182=PROPERTY_DEFINITION_REPRESENTATION(#11342,#11246);
#11183=PROPERTY_DEFINITION_REPRESENTATION(#11343,#11247);
#11184=PROPERTY_DEFINITION_REPRESENTATION(#11344,#11248);
#11185=PROPERTY_DEFINITION_REPRESENTATION(#11345,#11249);
#11186=PROPERTY_DEFINITION_REPRESENTATION(#11346,#11250);
#11187=PROPERTY_DEFINITION_REPRESENTATION(#11347,#11251);
#11188=PROPERTY_DEFINITION_REPRESENTATION(#11348,#11252);
#11189=PROPERTY_DEFINITION_REPRESENTATION(#11349,#11253);
#11190=PROPERTY_DEFINITION_REPRESENTATION(#11350,#11254);
#11191=PROPERTY_DEFINITION_REPRESENTATION(#11351,#11255);
#11192=PROPERTY_DEFINITION_REPRESENTATION(#11352,#11256);
#11193=PROPERTY_DEFINITION_REPRESENTATION(#11353,#11257);
#11194=PROPERTY_DEFINITION_REPRESENTATION(#11354,#11258);
#11195=PROPERTY_DEFINITION_REPRESENTATION(#11355,#11259);
#11196=PROPERTY_DEFINITION_REPRESENTATION(#11356,#11260);
#11197=PROPERTY_DEFINITION_REPRESENTATION(#11357,#11261);
#11198=PROPERTY_DEFINITION_REPRESENTATION(#11358,#11262);
#11199=PROPERTY_DEFINITION_REPRESENTATION(#11359,#11263);
#11200=PROPERTY_DEFINITION_REPRESENTATION(#11360,#11264);
#11201=PROPERTY_DEFINITION_REPRESENTATION(#11361,#11265);
#11202=PROPERTY_DEFINITION_REPRESENTATION(#11362,#11266);
#11203=PROPERTY_DEFINITION_REPRESENTATION(#11363,#11267);
#11204=PROPERTY_DEFINITION_REPRESENTATION(#11364,#11268);
#11205=PROPERTY_DEFINITION_REPRESENTATION(#11365,#11269);
#11206=PROPERTY_DEFINITION_REPRESENTATION(#11366,#11270);
#11207=PROPERTY_DEFINITION_REPRESENTATION(#11367,#11271);
#11208=PROPERTY_DEFINITION_REPRESENTATION(#11368,#11272);
#11209=PROPERTY_DEFINITION_REPRESENTATION(#11369,#11273);
#11210=PROPERTY_DEFINITION_REPRESENTATION(#11370,#11274);
#11211=PROPERTY_DEFINITION_REPRESENTATION(#11371,#11275);
#11212=PROPERTY_DEFINITION_REPRESENTATION(#11372,#11276);
#11213=REPRESENTATION('material name',(#11277),#19326);
#11214=REPRESENTATION('density',(#11117),#19326);
#11215=REPRESENTATION('material name',(#11278),#19327);
#11216=REPRESENTATION('density',(#11118),#19327);
#11217=REPRESENTATION('material name',(#11279),#19328);
#11218=REPRESENTATION('density',(#11119),#19328);
#11219=REPRESENTATION('material name',(#11280),#19329);
#11220=REPRESENTATION('density',(#11120),#19329);
#11221=REPRESENTATION('material name',(#11281),#19330);
#11222=REPRESENTATION('density',(#11121),#19330);
#11223=REPRESENTATION('material name',(#11282),#19331);
#11224=REPRESENTATION('density',(#11122),#19331);
#11225=REPRESENTATION('material name',(#11283),#19332);
#11226=REPRESENTATION('density',(#11123),#19332);
#11227=REPRESENTATION('material name',(#11284),#19333);
#11228=REPRESENTATION('density',(#11124),#19333);
#11229=REPRESENTATION('material name',(#11285),#19334);
#11230=REPRESENTATION('density',(#11125),#19334);
#11231=REPRESENTATION('material name',(#11286),#19335);
#11232=REPRESENTATION('density',(#11126),#19335);
#11233=REPRESENTATION('material name',(#11287),#19336);
#11234=REPRESENTATION('density',(#11127),#19336);
#11235=REPRESENTATION('material name',(#11288),#19337);
#11236=REPRESENTATION('density',(#11128),#19337);
#11237=REPRESENTATION('material name',(#11289),#19338);
#11238=REPRESENTATION('density',(#11129),#19338);
#11239=REPRESENTATION('material name',(#11290),#19340);
#11240=REPRESENTATION('density',(#11130),#19340);
#11241=REPRESENTATION('material name',(#11291),#19341);
#11242=REPRESENTATION('density',(#11131),#19341);
#11243=REPRESENTATION('material name',(#11292),#19342);
#11244=REPRESENTATION('density',(#11132),#19342);
#11245=REPRESENTATION('material name',(#11293),#19343);
#11246=REPRESENTATION('density',(#11133),#19343);
#11247=REPRESENTATION('material name',(#11294),#19344);
#11248=REPRESENTATION('density',(#11134),#19344);
#11249=REPRESENTATION('material name',(#11295),#19346);
#11250=REPRESENTATION('density',(#11135),#19346);
#11251=REPRESENTATION('material name',(#11296),#19347);
#11252=REPRESENTATION('density',(#11136),#19347);
#11253=REPRESENTATION('material name',(#11297),#19348);
#11254=REPRESENTATION('density',(#11137),#19348);
#11255=REPRESENTATION('material name',(#11298),#19349);
#11256=REPRESENTATION('density',(#11138),#19349);
#11257=REPRESENTATION('material name',(#11299),#19350);
#11258=REPRESENTATION('density',(#11139),#19350);
#11259=REPRESENTATION('material name',(#11300),#19351);
#11260=REPRESENTATION('density',(#11140),#19351);
#11261=REPRESENTATION('material name',(#11301),#19352);
#11262=REPRESENTATION('density',(#11141),#19352);
#11263=REPRESENTATION('material name',(#11302),#19353);
#11264=REPRESENTATION('density',(#11142),#19353);
#11265=REPRESENTATION('material name',(#11303),#19355);
#11266=REPRESENTATION('density',(#11143),#19355);
#11267=REPRESENTATION('material name',(#11304),#19356);
#11268=REPRESENTATION('density',(#11144),#19356);
#11269=REPRESENTATION('material name',(#11305),#19357);
#11270=REPRESENTATION('density',(#11145),#19357);
#11271=REPRESENTATION('material name',(#11306),#19358);
#11272=REPRESENTATION('density',(#11146),#19358);
#11273=REPRESENTATION('material name',(#11307),#19359);
#11274=REPRESENTATION('density',(#11147),#19359);
#11275=REPRESENTATION('material name',(#11308),#19360);
#11276=REPRESENTATION('density',(#11148),#19360);
#11277=DESCRIPTIVE_REPRESENTATION_ITEM('Steel','Steel');
#11278=DESCRIPTIVE_REPRESENTATION_ITEM('Steel','Steel');
#11279=DESCRIPTIVE_REPRESENTATION_ITEM('Steel','Steel');
#11280=DESCRIPTIVE_REPRESENTATION_ITEM('Steel','Steel');
#11281=DESCRIPTIVE_REPRESENTATION_ITEM('Steel','Steel');
#11282=DESCRIPTIVE_REPRESENTATION_ITEM('Steel','Steel');
#11283=DESCRIPTIVE_REPRESENTATION_ITEM('Steel','Steel');
#11284=DESCRIPTIVE_REPRESENTATION_ITEM('Steel','Steel');
#11285=DESCRIPTIVE_REPRESENTATION_ITEM('Steel','Steel');
#11286=DESCRIPTIVE_REPRESENTATION_ITEM('Steel','Steel');
#11287=DESCRIPTIVE_REPRESENTATION_ITEM('Steel','Steel');
#11288=DESCRIPTIVE_REPRESENTATION_ITEM('Steel','Steel');
#11289=DESCRIPTIVE_REPRESENTATION_ITEM('Steel','Steel');
#11290=DESCRIPTIVE_REPRESENTATION_ITEM('Steel','Steel');
#11291=DESCRIPTIVE_REPRESENTATION_ITEM('Steel','Steel');
#11292=DESCRIPTIVE_REPRESENTATION_ITEM('Steel','Steel');
#11293=DESCRIPTIVE_REPRESENTATION_ITEM('Steel','Steel');
#11294=DESCRIPTIVE_REPRESENTATION_ITEM('Steel','Steel');
#11295=DESCRIPTIVE_REPRESENTATION_ITEM('Steel','Steel');
#11296=DESCRIPTIVE_REPRESENTATION_ITEM('Steel','Steel');
#11297=DESCRIPTIVE_REPRESENTATION_ITEM('Steel','Steel');
#11298=DESCRIPTIVE_REPRESENTATION_ITEM('Steel','Steel');
#11299=DESCRIPTIVE_REPRESENTATION_ITEM('Steel','Steel');
#11300=DESCRIPTIVE_REPRESENTATION_ITEM('Steel','Steel');
#11301=DESCRIPTIVE_REPRESENTATION_ITEM('Steel','Steel');
#11302=DESCRIPTIVE_REPRESENTATION_ITEM('Steel','Steel');
#11303=DESCRIPTIVE_REPRESENTATION_ITEM('Steel','Steel');
#11304=DESCRIPTIVE_REPRESENTATION_ITEM('Steel','Steel');
#11305=DESCRIPTIVE_REPRESENTATION_ITEM('Steel','Steel');
#11306=DESCRIPTIVE_REPRESENTATION_ITEM('Steel','Steel');
#11307=DESCRIPTIVE_REPRESENTATION_ITEM('Steel','Steel');
#11308=DESCRIPTIVE_REPRESENTATION_ITEM('Steel','Steel');
#11309=PROPERTY_DEFINITION('material property','material name',#19528);
#11310=PROPERTY_DEFINITION('material property','density of part',#19528);
#11311=PROPERTY_DEFINITION('material property','material name',#19529);
#11312=PROPERTY_DEFINITION('material property','density of part',#19529);
#11313=PROPERTY_DEFINITION('material property','material name',#19530);
#11314=PROPERTY_DEFINITION('material property','density of part',#19530);
#11315=PROPERTY_DEFINITION('material property','material name',#19531);
#11316=PROPERTY_DEFINITION('material property','density of part',#19531);
#11317=PROPERTY_DEFINITION('material property','material name',#19532);
#11318=PROPERTY_DEFINITION('material property','density of part',#19532);
#11319=PROPERTY_DEFINITION('material property','material name',#19533);
#11320=PROPERTY_DEFINITION('material property','density of part',#19533);
#11321=PROPERTY_DEFINITION('material property','material name',#19534);
#11322=PROPERTY_DEFINITION('material property','density of part',#19534);
#11323=PROPERTY_DEFINITION('material property','material name',#19535);
#11324=PROPERTY_DEFINITION('material property','density of part',#19535);
#11325=PROPERTY_DEFINITION('material property','material name',#19536);
#11326=PROPERTY_DEFINITION('material property','density of part',#19536);
#11327=PROPERTY_DEFINITION('material property','material name',#19537);
#11328=PROPERTY_DEFINITION('material property','density of part',#19537);
#11329=PROPERTY_DEFINITION('material property','material name',#19538);
#11330=PROPERTY_DEFINITION('material property','density of part',#19538);
#11331=PROPERTY_DEFINITION('material property','material name',#19539);
#11332=PROPERTY_DEFINITION('material property','density of part',#19539);
#11333=PROPERTY_DEFINITION('material property','material name',#19540);
#11334=PROPERTY_DEFINITION('material property','density of part',#19540);
#11335=PROPERTY_DEFINITION('material property','material name',#19542);
#11336=PROPERTY_DEFINITION('material property','density of part',#19542);
#11337=PROPERTY_DEFINITION('material property','material name',#19543);
#11338=PROPERTY_DEFINITION('material property','density of part',#19543);
#11339=PROPERTY_DEFINITION('material property','material name',#19544);
#11340=PROPERTY_DEFINITION('material property','density of part',#19544);
#11341=PROPERTY_DEFINITION('material property','material name',#19545);
#11342=PROPERTY_DEFINITION('material property','density of part',#19545);
#11343=PROPERTY_DEFINITION('material property','material name',#19546);
#11344=PROPERTY_DEFINITION('material property','density of part',#19546);
#11345=PROPERTY_DEFINITION('material property','material name',#19548);
#11346=PROPERTY_DEFINITION('material property','density of part',#19548);
#11347=PROPERTY_DEFINITION('material property','material name',#19549);
#11348=PROPERTY_DEFINITION('material property','density of part',#19549);
#11349=PROPERTY_DEFINITION('material property','material name',#19550);
#11350=PROPERTY_DEFINITION('material property','density of part',#19550);
#11351=PROPERTY_DEFINITION('material property','material name',#19551);
#11352=PROPERTY_DEFINITION('material property','density of part',#19551);
#11353=PROPERTY_DEFINITION('material property','material name',#19552);
#11354=PROPERTY_DEFINITION('material property','density of part',#19552);
#11355=PROPERTY_DEFINITION('material property','material name',#19553);
#11356=PROPERTY_DEFINITION('material property','density of part',#19553);
#11357=PROPERTY_DEFINITION('material property','material name',#19554);
#11358=PROPERTY_DEFINITION('material property','density of part',#19554);
#11359=PROPERTY_DEFINITION('material property','material name',#19555);
#11360=PROPERTY_DEFINITION('material property','density of part',#19555);
#11361=PROPERTY_DEFINITION('material property','material name',#19557);
#11362=PROPERTY_DEFINITION('material property','density of part',#19557);
#11363=PROPERTY_DEFINITION('material property','material name',#19558);
#11364=PROPERTY_DEFINITION('material property','density of part',#19558);
#11365=PROPERTY_DEFINITION('material property','material name',#19559);
#11366=PROPERTY_DEFINITION('material property','density of part',#19559);
#11367=PROPERTY_DEFINITION('material property','material name',#19560);
#11368=PROPERTY_DEFINITION('material property','density of part',#19560);
#11369=PROPERTY_DEFINITION('material property','material name',#19561);
#11370=PROPERTY_DEFINITION('material property','density of part',#19561);
#11371=PROPERTY_DEFINITION('material property','material name',#19562);
#11372=PROPERTY_DEFINITION('material property','density of part',#19562);
#11373=AXIS2_PLACEMENT_3D('',#15427,#12340,#12341);
#11374=AXIS2_PLACEMENT_3D('',#15428,#12342,#12343);
#11375=AXIS2_PLACEMENT_3D('',#15429,#12344,#12345);
#11376=AXIS2_PLACEMENT_3D('',#15430,#12346,#12347);
#11377=AXIS2_PLACEMENT_3D('',#15432,#12348,#12349);
#11378=AXIS2_PLACEMENT_3D('',#15435,#12351,#12352);
#11379=AXIS2_PLACEMENT_3D('',#15436,#12353,#12354);
#11380=AXIS2_PLACEMENT_3D('',#15438,#12355,#12356);
#11381=AXIS2_PLACEMENT_3D('',#15441,#12358,#12359);
#11382=AXIS2_PLACEMENT_3D('',#15442,#12360,#12361);
#11383=AXIS2_PLACEMENT_3D('',#15444,#12362,#12363);
#11384=AXIS2_PLACEMENT_3D('',#15447,#12365,#12366);
#11385=AXIS2_PLACEMENT_3D('',#15448,#12367,#12368);
#11386=AXIS2_PLACEMENT_3D('',#15450,#12369,#12370);
#11387=AXIS2_PLACEMENT_3D('',#15453,#12372,#12373);
#11388=AXIS2_PLACEMENT_3D('',#15454,#12374,#12375);
#11389=AXIS2_PLACEMENT_3D('',#15456,#12376,#12377);
#11390=AXIS2_PLACEMENT_3D('',#15459,#12379,#12380);
#11391=AXIS2_PLACEMENT_3D('',#15460,#12381,#12382);
#11392=AXIS2_PLACEMENT_3D('',#15462,#12383,#12384);
#11393=AXIS2_PLACEMENT_3D('',#15465,#12386,#12387);
#11394=AXIS2_PLACEMENT_3D('',#15466,#12388,#12389);
#11395=AXIS2_PLACEMENT_3D('',#15475,#12394,#12395);
#11396=AXIS2_PLACEMENT_3D('',#15481,#12399,#12400);
#11397=AXIS2_PLACEMENT_3D('',#15487,#12404,#12405);
#11398=AXIS2_PLACEMENT_3D('',#15490,#12408,#12409);
#11399=AXIS2_PLACEMENT_3D('',#15491,#12410,#12411);
#11400=AXIS2_PLACEMENT_3D('',#15492,#12412,#12413);
#11401=AXIS2_PLACEMENT_3D('',#15493,#12414,#12415);
#11402=AXIS2_PLACEMENT_3D('',#15502,#12420,#12421);
#11403=AXIS2_PLACEMENT_3D('',#15508,#12425,#12426);
#11404=AXIS2_PLACEMENT_3D('',#15514,#12430,#12431);
#11405=AXIS2_PLACEMENT_3D('',#15517,#12434,#12435);
#11406=AXIS2_PLACEMENT_3D('',#15518,#12436,#12437);
#11407=AXIS2_PLACEMENT_3D('',#15519,#12438,#12439);
#11408=AXIS2_PLACEMENT_3D('',#15520,#12440,#12441);
#11409=AXIS2_PLACEMENT_3D('',#15529,#12446,#12447);
#11410=AXIS2_PLACEMENT_3D('',#15535,#12451,#12452);
#11411=AXIS2_PLACEMENT_3D('',#15541,#12456,#12457);
#11412=AXIS2_PLACEMENT_3D('',#15544,#12460,#12461);
#11413=AXIS2_PLACEMENT_3D('',#15545,#12462,#12463);
#11414=AXIS2_PLACEMENT_3D('',#15546,#12464,#12465);
#11415=AXIS2_PLACEMENT_3D('',#15547,#12466,#12467);
#11416=AXIS2_PLACEMENT_3D('',#15549,#12468,#12469);
#11417=AXIS2_PLACEMENT_3D('',#15552,#12471,#12472);
#11418=AXIS2_PLACEMENT_3D('',#15553,#12473,#12474);
#11419=AXIS2_PLACEMENT_3D('',#15555,#12475,#12476);
#11420=AXIS2_PLACEMENT_3D('',#15558,#12478,#12479);
#11421=AXIS2_PLACEMENT_3D('',#15559,#12480,#12481);
#11422=AXIS2_PLACEMENT_3D('',#15560,#12482,#12483);
#11423=AXIS2_PLACEMENT_3D('',#15561,#12484,#12485);
#11424=AXIS2_PLACEMENT_3D('',#15562,#12486,#12487);
#11425=AXIS2_PLACEMENT_3D('',#15564,#12488,#12489);
#11426=AXIS2_PLACEMENT_3D('',#15567,#12491,#12492);
#11427=AXIS2_PLACEMENT_3D('',#15568,#12493,#12494);
#11428=AXIS2_PLACEMENT_3D('',#15570,#12495,#12496);
#11429=AXIS2_PLACEMENT_3D('',#15573,#12498,#12499);
#11430=AXIS2_PLACEMENT_3D('',#15574,#12500,#12501);
#11431=AXIS2_PLACEMENT_3D('',#15575,#12502,#12503);
#11432=AXIS2_PLACEMENT_3D('',#15576,#12504,#12505);
#11433=AXIS2_PLACEMENT_3D('',#15577,#12506,#12507);
#11434=AXIS2_PLACEMENT_3D('',#15579,#12508,#12509);
#11435=AXIS2_PLACEMENT_3D('',#15582,#12511,#12512);
#11436=AXIS2_PLACEMENT_3D('',#15583,#12513,#12514);
#11437=AXIS2_PLACEMENT_3D('',#15585,#12515,#12516);
#11438=AXIS2_PLACEMENT_3D('',#15588,#12518,#12519);
#11439=AXIS2_PLACEMENT_3D('',#15589,#12520,#12521);
#11440=AXIS2_PLACEMENT_3D('',#15590,#12522,#12523);
#11441=AXIS2_PLACEMENT_3D('',#15591,#12524,#12525);
#11442=AXIS2_PLACEMENT_3D('',#15592,#12526,#12527);
#11443=AXIS2_PLACEMENT_3D('',#15594,#12528,#12529);
#11444=AXIS2_PLACEMENT_3D('',#15597,#12531,#12532);
#11445=AXIS2_PLACEMENT_3D('',#15598,#12533,#12534);
#11446=AXIS2_PLACEMENT_3D('',#15600,#12535,#12536);
#11447=AXIS2_PLACEMENT_3D('',#15603,#12538,#12539);
#11448=AXIS2_PLACEMENT_3D('',#15604,#12540,#12541);
#11449=AXIS2_PLACEMENT_3D('',#15605,#12542,#12543);
#11450=AXIS2_PLACEMENT_3D('',#15606,#12544,#12545);
#11451=AXIS2_PLACEMENT_3D('',#15607,#12546,#12547);
#11452=AXIS2_PLACEMENT_3D('',#15609,#12548,#12549);
#11453=AXIS2_PLACEMENT_3D('',#15612,#12551,#12552);
#11454=AXIS2_PLACEMENT_3D('',#15613,#12553,#12554);
#11455=AXIS2_PLACEMENT_3D('',#15615,#12555,#12556);
#11456=AXIS2_PLACEMENT_3D('',#15618,#12558,#12559);
#11457=AXIS2_PLACEMENT_3D('',#15619,#12560,#12561);
#11458=AXIS2_PLACEMENT_3D('',#15621,#12562,#12563);
#11459=AXIS2_PLACEMENT_3D('',#15624,#12565,#12566);
#11460=AXIS2_PLACEMENT_3D('',#15625,#12567,#12568);
#11461=AXIS2_PLACEMENT_3D('',#15627,#12569,#12570);
#11462=AXIS2_PLACEMENT_3D('',#15630,#12572,#12573);
#11463=AXIS2_PLACEMENT_3D('',#15631,#12574,#12575);
#11464=AXIS2_PLACEMENT_3D('',#15633,#12576,#12577);
#11465=AXIS2_PLACEMENT_3D('',#15636,#12579,#12580);
#11466=AXIS2_PLACEMENT_3D('',#15637,#12581,#12582);
#11467=AXIS2_PLACEMENT_3D('',#15639,#12583,#12584);
#11468=AXIS2_PLACEMENT_3D('',#15642,#12586,#12587);
#11469=AXIS2_PLACEMENT_3D('',#15643,#12588,#12589);
#11470=AXIS2_PLACEMENT_3D('',#15645,#12590,#12591);
#11471=AXIS2_PLACEMENT_3D('',#15648,#12593,#12594);
#11472=AXIS2_PLACEMENT_3D('',#15649,#12595,#12596);
#11473=AXIS2_PLACEMENT_3D('',#15658,#12601,#12602);
#11474=AXIS2_PLACEMENT_3D('',#15664,#12606,#12607);
#11475=AXIS2_PLACEMENT_3D('',#15673,#12612,#12613);
#11476=AXIS2_PLACEMENT_3D('',#15678,#12617,#12618);
#11477=AXIS2_PLACEMENT_3D('',#15683,#12622,#12623);
#11478=AXIS2_PLACEMENT_3D('',#15685,#12625,#12626);
#11479=AXIS2_PLACEMENT_3D('',#15686,#12627,#12628);
#11480=AXIS2_PLACEMENT_3D('',#15687,#12629,#12630);
#11481=AXIS2_PLACEMENT_3D('',#15688,#12631,#12632);
#11482=AXIS2_PLACEMENT_3D('',#15690,#12633,#12634);
#11483=AXIS2_PLACEMENT_3D('',#15693,#12636,#12637);
#11484=AXIS2_PLACEMENT_3D('',#15694,#12638,#12639);
#11485=AXIS2_PLACEMENT_3D('',#15695,#12640,#12641);
#11486=AXIS2_PLACEMENT_3D('',#15697,#12642,#12643);
#11487=AXIS2_PLACEMENT_3D('',#15700,#12645,#12646);
#11488=AXIS2_PLACEMENT_3D('',#15701,#12647,#12648);
#11489=AXIS2_PLACEMENT_3D('',#15702,#12649,#12650);
#11490=AXIS2_PLACEMENT_3D('',#15704,#12651,#12652);
#11491=AXIS2_PLACEMENT_3D('',#15707,#12654,#12655);
#11492=AXIS2_PLACEMENT_3D('',#15708,#12656,#12657);
#11493=AXIS2_PLACEMENT_3D('',#15709,#12658,#12659);
#11494=AXIS2_PLACEMENT_3D('',#15711,#12660,#12661);
#11495=AXIS2_PLACEMENT_3D('',#15714,#12663,#12664);
#11496=AXIS2_PLACEMENT_3D('',#15715,#12665,#12666);
#11497=AXIS2_PLACEMENT_3D('',#15716,#12667,#12668);
#11498=AXIS2_PLACEMENT_3D('',#15718,#12669,#12670);
#11499=AXIS2_PLACEMENT_3D('',#15721,#12672,#12673);
#11500=AXIS2_PLACEMENT_3D('',#15722,#12674,#12675);
#11501=AXIS2_PLACEMENT_3D('',#15724,#12676,#12677);
#11502=AXIS2_PLACEMENT_3D('',#15725,#12678,#12679);
#11503=AXIS2_PLACEMENT_3D('',#15727,#12680,#12681);
#11504=AXIS2_PLACEMENT_3D('',#15729,#12683,#12684);
#11505=AXIS2_PLACEMENT_3D('',#15738,#12689,#12690);
#11506=AXIS2_PLACEMENT_3D('',#15744,#12694,#12695);
#11507=AXIS2_PLACEMENT_3D('',#15750,#12699,#12700);
#11508=AXIS2_PLACEMENT_3D('',#15753,#12703,#12704);
#11509=AXIS2_PLACEMENT_3D('',#15754,#12705,#12706);
#11510=AXIS2_PLACEMENT_3D('',#15755,#12707,#12708);
#11511=AXIS2_PLACEMENT_3D('',#15756,#12709,#12710);
#11512=AXIS2_PLACEMENT_3D('',#15765,#12715,#12716);
#11513=AXIS2_PLACEMENT_3D('',#15771,#12720,#12721);
#11514=AXIS2_PLACEMENT_3D('',#15777,#12725,#12726);
#11515=AXIS2_PLACEMENT_3D('',#15783,#12730,#12731);
#11516=AXIS2_PLACEMENT_3D('',#15789,#12735,#12736);
#11517=AXIS2_PLACEMENT_3D('',#15792,#12739,#12740);
#11518=AXIS2_PLACEMENT_3D('',#15793,#12741,#12742);
#11519=AXIS2_PLACEMENT_3D('',#15795,#12743,#12744);
#11520=AXIS2_PLACEMENT_3D('',#15797,#12745,#12746);
#11521=AXIS2_PLACEMENT_3D('',#15798,#12747,#12748);
#11522=AXIS2_PLACEMENT_3D('',#15800,#12749,#12750);
#11523=AXIS2_PLACEMENT_3D('',#15802,#12752,#12753);
#11524=AXIS2_PLACEMENT_3D('',#15803,#12754,#12755);
#11525=AXIS2_PLACEMENT_3D('',#15806,#12757,#12758);
#11526=AXIS2_PLACEMENT_3D('',#15807,#12759,#12760);
#11527=AXIS2_PLACEMENT_3D('',#15808,#12761,#12762);
#11528=AXIS2_PLACEMENT_3D('',#15809,#12763,#12764);
#11529=AXIS2_PLACEMENT_3D('',#15818,#12769,#12770);
#11530=AXIS2_PLACEMENT_3D('',#15824,#12774,#12775);
#11531=AXIS2_PLACEMENT_3D('',#15830,#12779,#12780);
#11532=AXIS2_PLACEMENT_3D('',#15836,#12784,#12785);
#11533=AXIS2_PLACEMENT_3D('',#15842,#12789,#12790);
#11534=AXIS2_PLACEMENT_3D('',#15845,#12793,#12794);
#11535=AXIS2_PLACEMENT_3D('',#15846,#12795,#12796);
#11536=AXIS2_PLACEMENT_3D('',#15848,#12797,#12798);
#11537=AXIS2_PLACEMENT_3D('',#15850,#12799,#12800);
#11538=AXIS2_PLACEMENT_3D('',#15851,#12801,#12802);
#11539=AXIS2_PLACEMENT_3D('',#15853,#12803,#12804);
#11540=AXIS2_PLACEMENT_3D('',#15855,#12806,#12807);
#11541=AXIS2_PLACEMENT_3D('',#15856,#12808,#12809);
#11542=AXIS2_PLACEMENT_3D('',#15859,#12811,#12812);
#11543=AXIS2_PLACEMENT_3D('',#15860,#12813,#12814);
#11544=AXIS2_PLACEMENT_3D('',#15861,#12815,#12816);
#11545=AXIS2_PLACEMENT_3D('',#15862,#12817,#12818);
#11546=AXIS2_PLACEMENT_3D('',#15871,#12823,#12824);
#11547=AXIS2_PLACEMENT_3D('',#15877,#12828,#12829);
#11548=AXIS2_PLACEMENT_3D('',#15883,#12833,#12834);
#11549=AXIS2_PLACEMENT_3D('',#15889,#12838,#12839);
#11550=AXIS2_PLACEMENT_3D('',#15895,#12843,#12844);
#11551=AXIS2_PLACEMENT_3D('',#15898,#12847,#12848);
#11552=AXIS2_PLACEMENT_3D('',#15899,#12849,#12850);
#11553=AXIS2_PLACEMENT_3D('',#15901,#12851,#12852);
#11554=AXIS2_PLACEMENT_3D('',#15903,#12853,#12854);
#11555=AXIS2_PLACEMENT_3D('',#15904,#12855,#12856);
#11556=AXIS2_PLACEMENT_3D('',#15906,#12857,#12858);
#11557=AXIS2_PLACEMENT_3D('',#15908,#12860,#12861);
#11558=AXIS2_PLACEMENT_3D('',#15909,#12862,#12863);
#11559=AXIS2_PLACEMENT_3D('',#15912,#12865,#12866);
#11560=AXIS2_PLACEMENT_3D('',#15913,#12867,#12868);
#11561=AXIS2_PLACEMENT_3D('',#15914,#12869,#12870);
#11562=AXIS2_PLACEMENT_3D('',#15915,#12871,#12872);
#11563=AXIS2_PLACEMENT_3D('',#15924,#12877,#12878);
#11564=AXIS2_PLACEMENT_3D('',#15930,#12882,#12883);
#11565=AXIS2_PLACEMENT_3D('',#15936,#12887,#12888);
#11566=AXIS2_PLACEMENT_3D('',#15942,#12892,#12893);
#11567=AXIS2_PLACEMENT_3D('',#15948,#12897,#12898);
#11568=AXIS2_PLACEMENT_3D('',#15951,#12901,#12902);
#11569=AXIS2_PLACEMENT_3D('',#15952,#12903,#12904);
#11570=AXIS2_PLACEMENT_3D('',#15954,#12905,#12906);
#11571=AXIS2_PLACEMENT_3D('',#15956,#12907,#12908);
#11572=AXIS2_PLACEMENT_3D('',#15957,#12909,#12910);
#11573=AXIS2_PLACEMENT_3D('',#15959,#12911,#12912);
#11574=AXIS2_PLACEMENT_3D('',#15961,#12914,#12915);
#11575=AXIS2_PLACEMENT_3D('',#15962,#12916,#12917);
#11576=AXIS2_PLACEMENT_3D('',#15965,#12919,#12920);
#11577=AXIS2_PLACEMENT_3D('',#15966,#12921,#12922);
#11578=AXIS2_PLACEMENT_3D('',#15967,#12923,#12924);
#11579=AXIS2_PLACEMENT_3D('',#15968,#12925,#12926);
#11580=AXIS2_PLACEMENT_3D('',#15969,#12927,#12928);
#11581=AXIS2_PLACEMENT_3D('',#15973,#12930,#12931);
#11582=AXIS2_PLACEMENT_3D('',#15974,#12932,#12933);
#11583=AXIS2_PLACEMENT_3D('',#15979,#12935,#12936);
#11584=AXIS2_PLACEMENT_3D('',#15983,#12938,#12939);
#11585=AXIS2_PLACEMENT_3D('',#15986,#12941,#12942);
#11586=AXIS2_PLACEMENT_3D('',#15987,#12943,#12944);
#11587=AXIS2_PLACEMENT_3D('',#15988,#12945,#12946);
#11588=AXIS2_PLACEMENT_3D('',#15990,#12947,#12948);
#11589=AXIS2_PLACEMENT_3D('',#15994,#12950,#12951);
#11590=AXIS2_PLACEMENT_3D('',#15998,#12954,#12955);
#11591=AXIS2_PLACEMENT_3D('',#15999,#12956,#12957);
#11592=AXIS2_PLACEMENT_3D('',#16001,#12959,#12960);
#11593=AXIS2_PLACEMENT_3D('',#16005,#12962,#12963);
#11594=AXIS2_PLACEMENT_3D('',#16007,#12965,#12966);
#11595=AXIS2_PLACEMENT_3D('',#16010,#12967,#12968);
#11596=AXIS2_PLACEMENT_3D('',#16011,#12969,#12970);
#11597=AXIS2_PLACEMENT_3D('',#16017,#12973,#12974);
#11598=AXIS2_PLACEMENT_3D('',#16018,#12975,#12976);
#11599=AXIS2_PLACEMENT_3D('',#16023,#12978,#12979);
#11600=AXIS2_PLACEMENT_3D('',#16025,#12981,#12982);
#11601=AXIS2_PLACEMENT_3D('',#16030,#12984,#12985);
#11602=AXIS2_PLACEMENT_3D('',#16032,#12987,#12988);
#11603=AXIS2_PLACEMENT_3D('',#16035,#12991,#12992);
#11604=AXIS2_PLACEMENT_3D('',#16041,#12995,#12996);
#11605=AXIS2_PLACEMENT_3D('',#16042,#12997,#12998);
#11606=AXIS2_PLACEMENT_3D('',#16045,#13001,#13002);
#11607=AXIS2_PLACEMENT_3D('',#16063,#13013,#13014);
#11608=AXIS2_PLACEMENT_3D('',#16065,#13015,#13016);
#11609=AXIS2_PLACEMENT_3D('',#16066,#13017,#13018);
#11610=AXIS2_PLACEMENT_3D('',#16069,#13019,#13020);
#11611=AXIS2_PLACEMENT_3D('',#16073,#13022,#13023);
#11612=AXIS2_PLACEMENT_3D('',#16075,#13025,#13026);
#11613=AXIS2_PLACEMENT_3D('',#16076,#13027,#13028);
#11614=AXIS2_PLACEMENT_3D('',#16077,#13029,#13030);
#11615=AXIS2_PLACEMENT_3D('',#16078,#13031,#13032);
#11616=AXIS2_PLACEMENT_3D('',#16088,#13038,#13039);
#11617=AXIS2_PLACEMENT_3D('',#16092,#13042,#13043);
#11618=AXIS2_PLACEMENT_3D('',#16098,#13047,#13048);
#11619=AXIS2_PLACEMENT_3D('',#16103,#13052,#13053);
#11620=AXIS2_PLACEMENT_3D('',#16105,#13055,#13056);
#11621=AXIS2_PLACEMENT_3D('',#16106,#13057,#13058);
#11622=AXIS2_PLACEMENT_3D('',#16108,#13059,#13060);
#11623=AXIS2_PLACEMENT_3D('',#16110,#13062,#13063);
#11624=AXIS2_PLACEMENT_3D('',#16112,#13064,#13065);
#11625=AXIS2_PLACEMENT_3D('',#16114,#13067,#13068);
#11626=AXIS2_PLACEMENT_3D('',#16120,#13072,#13073);
#11627=AXIS2_PLACEMENT_3D('',#16124,#13076,#13077);
#11628=AXIS2_PLACEMENT_3D('',#16128,#13080,#13081);
#11629=AXIS2_PLACEMENT_3D('',#16130,#13083,#13084);
#11630=AXIS2_PLACEMENT_3D('',#16131,#13085,#13086);
#11631=AXIS2_PLACEMENT_3D('',#16132,#13087,#13088);
#11632=AXIS2_PLACEMENT_3D('',#16134,#13089,#13090);
#11633=AXIS2_PLACEMENT_3D('',#16137,#13092,#13093);
#11634=AXIS2_PLACEMENT_3D('',#16138,#13094,#13095);
#11635=AXIS2_PLACEMENT_3D('',#16140,#13096,#13097);
#11636=AXIS2_PLACEMENT_3D('',#16141,#13098,#13099);
#11637=AXIS2_PLACEMENT_3D('',#16144,#13100,#13101);
#11638=AXIS2_PLACEMENT_3D('',#16146,#13102,#13103);
#11639=AXIS2_PLACEMENT_3D('',#16147,#13104,#13105);
#11640=AXIS2_PLACEMENT_3D('',#16148,#13106,#13107);
#11641=AXIS2_PLACEMENT_3D('',#16226,#13109,#13110);
#11642=AXIS2_PLACEMENT_3D('',#16304,#13112,#13113);
#11643=AXIS2_PLACEMENT_3D('',#16306,#13114,#13115);
#11644=AXIS2_PLACEMENT_3D('',#16309,#13117,#13118);
#11645=AXIS2_PLACEMENT_3D('',#16474,#13119,#13120);
#11646=AXIS2_PLACEMENT_3D('',#16511,#13122,#13123);
#11647=AXIS2_PLACEMENT_3D('',#16548,#13125,#13126);
#11648=AXIS2_PLACEMENT_3D('',#16585,#13128,#13129);
#11649=AXIS2_PLACEMENT_3D('',#16622,#13131,#13132);
#11650=AXIS2_PLACEMENT_3D('',#16624,#13133,#13134);
#11651=AXIS2_PLACEMENT_3D('',#16625,#13135,#13136);
#11652=AXIS2_PLACEMENT_3D('',#16627,#13137,#13138);
#11653=AXIS2_PLACEMENT_3D('',#16628,#13139,#13140);
#11654=AXIS2_PLACEMENT_3D('',#16630,#13141,#13142);
#11655=AXIS2_PLACEMENT_3D('',#16632,#13144,#13145);
#11656=AXIS2_PLACEMENT_3D('',#16634,#13146,#13147);
#11657=AXIS2_PLACEMENT_3D('',#16635,#13148,#13149);
#11658=AXIS2_PLACEMENT_3D('',#16637,#13151,#13152);
#11659=AXIS2_PLACEMENT_3D('',#16638,#13153,#13154);
#11660=AXIS2_PLACEMENT_3D('',#16639,#13155,#13156);
#11661=AXIS2_PLACEMENT_3D('',#16640,#13157,#13158);
#11662=AXIS2_PLACEMENT_3D('',#16642,#13159,#13160);
#11663=AXIS2_PLACEMENT_3D('',#16645,#13162,#13163);
#11664=AXIS2_PLACEMENT_3D('',#16646,#13164,#13165);
#11665=AXIS2_PLACEMENT_3D('',#16648,#13166,#13167);
#11666=AXIS2_PLACEMENT_3D('',#16651,#13169,#13170);
#11667=AXIS2_PLACEMENT_3D('',#16652,#13171,#13172);
#11668=AXIS2_PLACEMENT_3D('',#16653,#13173,#13174);
#11669=AXIS2_PLACEMENT_3D('',#16654,#13175,#13176);
#11670=AXIS2_PLACEMENT_3D('',#16655,#13177,#13178);
#11671=AXIS2_PLACEMENT_3D('',#16664,#13183,#13184);
#11672=AXIS2_PLACEMENT_3D('',#16670,#13188,#13189);
#11673=AXIS2_PLACEMENT_3D('',#16676,#13193,#13194);
#11674=AXIS2_PLACEMENT_3D('',#16682,#13198,#13199);
#11675=AXIS2_PLACEMENT_3D('',#16688,#13203,#13204);
#11676=AXIS2_PLACEMENT_3D('',#16691,#13207,#13208);
#11677=AXIS2_PLACEMENT_3D('',#16692,#13209,#13210);
#11678=AXIS2_PLACEMENT_3D('',#16693,#13211,#13212);
#11679=AXIS2_PLACEMENT_3D('',#16695,#13213,#13214);
#11680=AXIS2_PLACEMENT_3D('',#16696,#13215,#13216);
#11681=AXIS2_PLACEMENT_3D('',#16698,#13217,#13218);
#11682=AXIS2_PLACEMENT_3D('',#16699,#13219,#13220);
#11683=AXIS2_PLACEMENT_3D('',#16701,#13221,#13222);
#11684=AXIS2_PLACEMENT_3D('',#16703,#13224,#13225);
#11685=AXIS2_PLACEMENT_3D('',#16705,#13226,#13227);
#11686=AXIS2_PLACEMENT_3D('',#16707,#13229,#13230);
#11687=AXIS2_PLACEMENT_3D('',#16709,#13231,#13232);
#11688=AXIS2_PLACEMENT_3D('',#16711,#13234,#13235);
#11689=AXIS2_PLACEMENT_3D('',#16713,#13236,#13237);
#11690=AXIS2_PLACEMENT_3D('',#16714,#13238,#13239);
#11691=AXIS2_PLACEMENT_3D('',#16716,#13240,#13241);
#11692=AXIS2_PLACEMENT_3D('',#16718,#13243,#13244);
#11693=AXIS2_PLACEMENT_3D('',#16720,#13246,#13247);
#11694=AXIS2_PLACEMENT_3D('',#16721,#13248,#13249);
#11695=AXIS2_PLACEMENT_3D('',#16730,#13254,#13255);
#11696=AXIS2_PLACEMENT_3D('',#16736,#13259,#13260);
#11697=AXIS2_PLACEMENT_3D('',#16742,#13264,#13265);
#11698=AXIS2_PLACEMENT_3D('',#16748,#13269,#13270);
#11699=AXIS2_PLACEMENT_3D('',#16754,#13274,#13275);
#11700=AXIS2_PLACEMENT_3D('',#16757,#13278,#13279);
#11701=AXIS2_PLACEMENT_3D('',#16758,#13280,#13281);
#11702=AXIS2_PLACEMENT_3D('',#16759,#13282,#13283);
#11703=AXIS2_PLACEMENT_3D('',#16761,#13284,#13285);
#11704=AXIS2_PLACEMENT_3D('',#16762,#13286,#13287);
#11705=AXIS2_PLACEMENT_3D('',#16764,#13288,#13289);
#11706=AXIS2_PLACEMENT_3D('',#16765,#13290,#13291);
#11707=AXIS2_PLACEMENT_3D('',#16767,#13292,#13293);
#11708=AXIS2_PLACEMENT_3D('',#16769,#13295,#13296);
#11709=AXIS2_PLACEMENT_3D('',#16771,#13297,#13298);
#11710=AXIS2_PLACEMENT_3D('',#16773,#13300,#13301);
#11711=AXIS2_PLACEMENT_3D('',#16775,#13302,#13303);
#11712=AXIS2_PLACEMENT_3D('',#16777,#13305,#13306);
#11713=AXIS2_PLACEMENT_3D('',#16779,#13307,#13308);
#11714=AXIS2_PLACEMENT_3D('',#16780,#13309,#13310);
#11715=AXIS2_PLACEMENT_3D('',#16782,#13311,#13312);
#11716=AXIS2_PLACEMENT_3D('',#16784,#13314,#13315);
#11717=AXIS2_PLACEMENT_3D('',#16786,#13317,#13318);
#11718=AXIS2_PLACEMENT_3D('',#16787,#13319,#13320);
#11719=AXIS2_PLACEMENT_3D('',#16788,#13321,#13322);
#11720=AXIS2_PLACEMENT_3D('',#16789,#13323,#13324);
#11721=AXIS2_PLACEMENT_3D('',#16790,#13325,#13326);
#11722=AXIS2_PLACEMENT_3D('',#16791,#13327,#13328);
#11723=AXIS2_PLACEMENT_3D('',#16792,#13329,#13330);
#11724=AXIS2_PLACEMENT_3D('',#16793,#13331,#13332);
#11725=AXIS2_PLACEMENT_3D('',#16794,#13333,#13334);
#11726=AXIS2_PLACEMENT_3D('',#16795,#13335,#13336);
#11727=AXIS2_PLACEMENT_3D('',#16796,#13337,#13338);
#11728=AXIS2_PLACEMENT_3D('',#16797,#13339,#13340);
#11729=AXIS2_PLACEMENT_3D('',#16798,#13341,#13342);
#11730=AXIS2_PLACEMENT_3D('',#16799,#13343,#13344);
#11731=AXIS2_PLACEMENT_3D('',#16800,#13345,#13346);
#11732=AXIS2_PLACEMENT_3D('',#16801,#13347,#13348);
#11733=AXIS2_PLACEMENT_3D('',#16802,#13349,#13350);
#11734=AXIS2_PLACEMENT_3D('',#16803,#13351,#13352);
#11735=AXIS2_PLACEMENT_3D('',#16804,#13353,#13354);
#11736=AXIS2_PLACEMENT_3D('',#16805,#13355,#13356);
#11737=AXIS2_PLACEMENT_3D('',#16806,#13357,#13358);
#11738=AXIS2_PLACEMENT_3D('',#16807,#13359,#13360);
#11739=AXIS2_PLACEMENT_3D('',#16808,#13361,#13362);
#11740=AXIS2_PLACEMENT_3D('',#16809,#13363,#13364);
#11741=AXIS2_PLACEMENT_3D('',#16810,#13365,#13366);
#11742=AXIS2_PLACEMENT_3D('',#16811,#13367,#13368);
#11743=AXIS2_PLACEMENT_3D('',#16812,#13369,#13370);
#11744=AXIS2_PLACEMENT_3D('',#16813,#13371,#13372);
#11745=AXIS2_PLACEMENT_3D('',#16822,#13377,#13378);
#11746=AXIS2_PLACEMENT_3D('',#16824,#13379,#13380);
#11747=AXIS2_PLACEMENT_3D('',#16828,#13383,#13384);
#11748=AXIS2_PLACEMENT_3D('',#16834,#13388,#13389);
#11749=AXIS2_PLACEMENT_3D('',#16836,#13391,#13392);
#11750=AXIS2_PLACEMENT_3D('',#16837,#13393,#13394);
#11751=AXIS2_PLACEMENT_3D('',#16838,#13395,#13396);
#11752=AXIS2_PLACEMENT_3D('',#16840,#13397,#13398);
#11753=AXIS2_PLACEMENT_3D('',#16843,#13400,#13401);
#11754=AXIS2_PLACEMENT_3D('',#16844,#13402,#13403);
#11755=AXIS2_PLACEMENT_3D('',#16845,#13404,#13405);
#11756=AXIS2_PLACEMENT_3D('',#16847,#13406,#13407);
#11757=AXIS2_PLACEMENT_3D('',#16850,#13409,#13410);
#11758=AXIS2_PLACEMENT_3D('',#16851,#13411,#13412);
#11759=AXIS2_PLACEMENT_3D('',#16852,#13413,#13414);
#11760=AXIS2_PLACEMENT_3D('',#16853,#13415,#13416);
#11761=AXIS2_PLACEMENT_3D('',#16854,#13417,#13418);
#11762=AXIS2_PLACEMENT_3D('',#16856,#13419,#13420);
#11763=AXIS2_PLACEMENT_3D('',#16859,#13422,#13423);
#11764=AXIS2_PLACEMENT_3D('',#16860,#13424,#13425);
#11765=AXIS2_PLACEMENT_3D('',#16861,#13426,#13427);
#11766=AXIS2_PLACEMENT_3D('',#16862,#13428,#13429);
#11767=AXIS2_PLACEMENT_3D('',#16863,#13430,#13431);
#11768=AXIS2_PLACEMENT_3D('',#16867,#13433,#13434);
#11769=AXIS2_PLACEMENT_3D('',#16868,#13435,#13436);
#11770=AXIS2_PLACEMENT_3D('',#16881,#13437,#13438);
#11771=AXIS2_PLACEMENT_3D('',#16922,#13440,#13441);
#11772=AXIS2_PLACEMENT_3D('',#16933,#13442,#13443);
#11773=AXIS2_PLACEMENT_3D('',#16935,#13445,#13446);
#11774=AXIS2_PLACEMENT_3D('',#16937,#13447,#13448);
#11775=AXIS2_PLACEMENT_3D('',#16940,#13450,#13451);
#11776=AXIS2_PLACEMENT_3D('',#16941,#13452,#13453);
#11777=AXIS2_PLACEMENT_3D('',#16943,#13454,#13455);
#11778=AXIS2_PLACEMENT_3D('',#16946,#13457,#13458);
#11779=AXIS2_PLACEMENT_3D('',#16947,#13459,#13460);
#11780=AXIS2_PLACEMENT_3D('',#16948,#13461,#13462);
#11781=AXIS2_PLACEMENT_3D('',#16949,#13463,#13464);
#11782=AXIS2_PLACEMENT_3D('',#16950,#13465,#13466);
#11783=AXIS2_PLACEMENT_3D('',#16954,#13468,#13469);
#11784=AXIS2_PLACEMENT_3D('',#16955,#13470,#13471);
#11785=AXIS2_PLACEMENT_3D('',#16968,#13472,#13473);
#11786=AXIS2_PLACEMENT_3D('',#17009,#13475,#13476);
#11787=AXIS2_PLACEMENT_3D('',#17020,#13477,#13478);
#11788=AXIS2_PLACEMENT_3D('',#17022,#13480,#13481);
#11789=AXIS2_PLACEMENT_3D('',#17031,#13486,#13487);
#11790=AXIS2_PLACEMENT_3D('',#17037,#13491,#13492);
#11791=AXIS2_PLACEMENT_3D('',#17043,#13496,#13497);
#11792=AXIS2_PLACEMENT_3D('',#17045,#13498,#13499);
#11793=AXIS2_PLACEMENT_3D('',#17046,#13500,#13501);
#11794=AXIS2_PLACEMENT_3D('',#17047,#13502,#13503);
#11795=AXIS2_PLACEMENT_3D('',#17048,#13504,#13505);
#11796=AXIS2_PLACEMENT_3D('',#17049,#13506,#13507);
#11797=AXIS2_PLACEMENT_3D('',#17051,#13508,#13509);
#11798=AXIS2_PLACEMENT_3D('',#17053,#13510,#13511);
#11799=AXIS2_PLACEMENT_3D('',#17054,#13512,#13513);
#11800=AXIS2_PLACEMENT_3D('',#17056,#13514,#13515);
#11801=AXIS2_PLACEMENT_3D('',#17058,#13516,#13517);
#11802=AXIS2_PLACEMENT_3D('',#17059,#13518,#13519);
#11803=AXIS2_PLACEMENT_3D('',#17061,#13521,#13522);
#11804=AXIS2_PLACEMENT_3D('',#17064,#13524,#13525);
#11805=AXIS2_PLACEMENT_3D('',#17065,#13526,#13527);
#11806=AXIS2_PLACEMENT_3D('',#17067,#13529,#13530);
#11807=AXIS2_PLACEMENT_3D('',#17068,#13531,#13532);
#11808=AXIS2_PLACEMENT_3D('',#17069,#13533,#13534);
#11809=AXIS2_PLACEMENT_3D('',#17073,#13536,#13537);
#11810=AXIS2_PLACEMENT_3D('',#17074,#13538,#13539);
#11811=AXIS2_PLACEMENT_3D('',#17087,#13540,#13541);
#11812=AXIS2_PLACEMENT_3D('',#17128,#13543,#13544);
#11813=AXIS2_PLACEMENT_3D('',#17139,#13545,#13546);
#11814=AXIS2_PLACEMENT_3D('',#17141,#13548,#13549);
#11815=AXIS2_PLACEMENT_3D('',#17143,#13550,#13551);
#11816=AXIS2_PLACEMENT_3D('',#17146,#13553,#13554);
#11817=AXIS2_PLACEMENT_3D('',#17147,#13555,#13556);
#11818=AXIS2_PLACEMENT_3D('',#17149,#13557,#13558);
#11819=AXIS2_PLACEMENT_3D('',#17152,#13560,#13561);
#11820=AXIS2_PLACEMENT_3D('',#17153,#13562,#13563);
#11821=AXIS2_PLACEMENT_3D('',#17154,#13564,#13565);
#11822=AXIS2_PLACEMENT_3D('',#17155,#13566,#13567);
#11823=AXIS2_PLACEMENT_3D('',#17156,#13568,#13569);
#11824=AXIS2_PLACEMENT_3D('',#17160,#13571,#13572);
#11825=AXIS2_PLACEMENT_3D('',#17161,#13573,#13574);
#11826=AXIS2_PLACEMENT_3D('',#17174,#13575,#13576);
#11827=AXIS2_PLACEMENT_3D('',#17215,#13578,#13579);
#11828=AXIS2_PLACEMENT_3D('',#17226,#13580,#13581);
#11829=AXIS2_PLACEMENT_3D('',#17228,#13583,#13584);
#11830=AXIS2_PLACEMENT_3D('',#17230,#13585,#13586);
#11831=AXIS2_PLACEMENT_3D('',#17233,#13588,#13589);
#11832=AXIS2_PLACEMENT_3D('',#17234,#13590,#13591);
#11833=AXIS2_PLACEMENT_3D('',#17236,#13592,#13593);
#11834=AXIS2_PLACEMENT_3D('',#17239,#13595,#13596);
#11835=AXIS2_PLACEMENT_3D('',#17240,#13597,#13598);
#11836=AXIS2_PLACEMENT_3D('',#17241,#13599,#13600);
#11837=AXIS2_PLACEMENT_3D('',#17242,#13601,#13602);
#11838=AXIS2_PLACEMENT_3D('',#17243,#13603,#13604);
#11839=AXIS2_PLACEMENT_3D('',#17245,#13605,#13606);
#11840=AXIS2_PLACEMENT_3D('',#17248,#13608,#13609);
#11841=AXIS2_PLACEMENT_3D('',#17249,#13610,#13611);
#11842=AXIS2_PLACEMENT_3D('',#17251,#13612,#13613);
#11843=AXIS2_PLACEMENT_3D('',#17254,#13615,#13616);
#11844=AXIS2_PLACEMENT_3D('',#17255,#13617,#13618);
#11845=AXIS2_PLACEMENT_3D('',#17256,#13619,#13620);
#11846=AXIS2_PLACEMENT_3D('',#17257,#13621,#13622);
#11847=AXIS2_PLACEMENT_3D('',#17258,#13623,#13624);
#11848=AXIS2_PLACEMENT_3D('',#17267,#13629,#13630);
#11849=AXIS2_PLACEMENT_3D('',#17273,#13634,#13635);
#11850=AXIS2_PLACEMENT_3D('',#17279,#13639,#13640);
#11851=AXIS2_PLACEMENT_3D('',#17285,#13644,#13645);
#11852=AXIS2_PLACEMENT_3D('',#17291,#13649,#13650);
#11853=AXIS2_PLACEMENT_3D('',#17294,#13653,#13654);
#11854=AXIS2_PLACEMENT_3D('',#17295,#13655,#13656);
#11855=AXIS2_PLACEMENT_3D('',#17297,#13657,#13658);
#11856=AXIS2_PLACEMENT_3D('',#17298,#13659,#13660);
#11857=AXIS2_PLACEMENT_3D('',#17300,#13661,#13662);
#11858=AXIS2_PLACEMENT_3D('',#17302,#13664,#13665);
#11859=AXIS2_PLACEMENT_3D('',#17304,#13666,#13667);
#11860=AXIS2_PLACEMENT_3D('',#17306,#13669,#13670);
#11861=AXIS2_PLACEMENT_3D('',#17308,#13671,#13672);
#11862=AXIS2_PLACEMENT_3D('',#17310,#13674,#13675);
#11863=AXIS2_PLACEMENT_3D('',#17311,#13676,#13677);
#11864=AXIS2_PLACEMENT_3D('',#17312,#13678,#13679);
#11865=AXIS2_PLACEMENT_3D('',#17313,#13680,#13681);
#11866=AXIS2_PLACEMENT_3D('',#17388,#13683,#13684);
#11867=AXIS2_PLACEMENT_3D('',#17390,#13685,#13686);
#11868=AXIS2_PLACEMENT_3D('',#17393,#13688,#13689);
#11869=AXIS2_PLACEMENT_3D('',#17394,#13690,#13691);
#11870=AXIS2_PLACEMENT_3D('',#17403,#13696,#13697);
#11871=AXIS2_PLACEMENT_3D('',#17409,#13701,#13702);
#11872=AXIS2_PLACEMENT_3D('',#17415,#13706,#13707);
#11873=AXIS2_PLACEMENT_3D('',#17421,#13711,#13712);
#11874=AXIS2_PLACEMENT_3D('',#17427,#13716,#13717);
#11875=AXIS2_PLACEMENT_3D('',#17433,#13721,#13722);
#11876=AXIS2_PLACEMENT_3D('',#17439,#13726,#13727);
#11877=AXIS2_PLACEMENT_3D('',#17445,#13731,#13732);
#11878=AXIS2_PLACEMENT_3D('',#17451,#13736,#13737);
#11879=AXIS2_PLACEMENT_3D('',#17457,#13741,#13742);
#11880=AXIS2_PLACEMENT_3D('',#17463,#13746,#13747);
#11881=AXIS2_PLACEMENT_3D('',#17469,#13751,#13752);
#11882=AXIS2_PLACEMENT_3D('',#17475,#13756,#13757);
#11883=AXIS2_PLACEMENT_3D('',#17481,#13761,#13762);
#11884=AXIS2_PLACEMENT_3D('',#17487,#13766,#13767);
#11885=AXIS2_PLACEMENT_3D('',#17493,#13771,#13772);
#11886=AXIS2_PLACEMENT_3D('',#17499,#13776,#13777);
#11887=AXIS2_PLACEMENT_3D('',#17502,#13780,#13781);
#11888=AXIS2_PLACEMENT_3D('',#17503,#13782,#13783);
#11889=AXIS2_PLACEMENT_3D('',#17504,#13784,#13785);
#11890=AXIS2_PLACEMENT_3D('',#17505,#13786,#13787);
#11891=AXIS2_PLACEMENT_3D('',#17506,#13788,#13789);
#11892=AXIS2_PLACEMENT_3D('',#17507,#13790,#13791);
#11893=AXIS2_PLACEMENT_3D('',#17508,#13792,#13793);
#11894=AXIS2_PLACEMENT_3D('',#17509,#13794,#13795);
#11895=AXIS2_PLACEMENT_3D('',#17510,#13796,#13797);
#11896=AXIS2_PLACEMENT_3D('',#17511,#13798,#13799);
#11897=AXIS2_PLACEMENT_3D('',#17512,#13800,#13801);
#11898=AXIS2_PLACEMENT_3D('',#17513,#13802,#13803);
#11899=AXIS2_PLACEMENT_3D('',#17514,#13804,#13805);
#11900=AXIS2_PLACEMENT_3D('',#17515,#13806,#13807);
#11901=AXIS2_PLACEMENT_3D('',#17516,#13808,#13809);
#11902=AXIS2_PLACEMENT_3D('',#17517,#13810,#13811);
#11903=AXIS2_PLACEMENT_3D('',#17518,#13812,#13813);
#11904=AXIS2_PLACEMENT_3D('',#17519,#13814,#13815);
#11905=AXIS2_PLACEMENT_3D('',#17521,#13816,#13817);
#11906=AXIS2_PLACEMENT_3D('',#17543,#13828,#13829);
#11907=AXIS2_PLACEMENT_3D('',#17565,#13840,#13841);
#11908=AXIS2_PLACEMENT_3D('',#17566,#13842,#13843);
#11909=AXIS2_PLACEMENT_3D('',#17567,#13844,#13845);
#11910=AXIS2_PLACEMENT_3D('',#17575,#13850,#13851);
#11911=AXIS2_PLACEMENT_3D('',#17581,#13855,#13856);
#11912=AXIS2_PLACEMENT_3D('',#17587,#13860,#13861);
#11913=AXIS2_PLACEMENT_3D('',#17593,#13865,#13866);
#11914=AXIS2_PLACEMENT_3D('',#17599,#13870,#13871);
#11915=AXIS2_PLACEMENT_3D('',#17605,#13875,#13876);
#11916=AXIS2_PLACEMENT_3D('',#17611,#13880,#13881);
#11917=AXIS2_PLACEMENT_3D('',#17616,#13885,#13886);
#11918=AXIS2_PLACEMENT_3D('',#17620,#13889,#13890);
#11919=AXIS2_PLACEMENT_3D('',#17624,#13893,#13894);
#11920=AXIS2_PLACEMENT_3D('',#17628,#13897,#13898);
#11921=AXIS2_PLACEMENT_3D('',#17632,#13901,#13902);
#11922=AXIS2_PLACEMENT_3D('',#17636,#13905,#13906);
#11923=AXIS2_PLACEMENT_3D('',#17640,#13909,#13910);
#11924=AXIS2_PLACEMENT_3D('',#17644,#13913,#13914);
#11925=AXIS2_PLACEMENT_3D('',#17648,#13917,#13918);
#11926=AXIS2_PLACEMENT_3D('',#17652,#13921,#13922);
#11927=AXIS2_PLACEMENT_3D('',#17654,#13924,#13925);
#11928=AXIS2_PLACEMENT_3D('',#17655,#13926,#13927);
#11929=AXIS2_PLACEMENT_3D('',#17656,#13928,#13929);
#11930=AXIS2_PLACEMENT_3D('',#17657,#13930,#13931);
#11931=AXIS2_PLACEMENT_3D('',#17658,#13932,#13933);
#11932=AXIS2_PLACEMENT_3D('',#17659,#13934,#13935);
#11933=AXIS2_PLACEMENT_3D('',#17660,#13936,#13937);
#11934=AXIS2_PLACEMENT_3D('',#17661,#13938,#13939);
#11935=AXIS2_PLACEMENT_3D('',#17662,#13940,#13941);
#11936=AXIS2_PLACEMENT_3D('',#17663,#13942,#13943);
#11937=AXIS2_PLACEMENT_3D('',#17664,#13944,#13945);
#11938=AXIS2_PLACEMENT_3D('',#17665,#13946,#13947);
#11939=AXIS2_PLACEMENT_3D('',#17666,#13948,#13949);
#11940=AXIS2_PLACEMENT_3D('',#17667,#13950,#13951);
#11941=AXIS2_PLACEMENT_3D('',#17668,#13952,#13953);
#11942=AXIS2_PLACEMENT_3D('',#17669,#13954,#13955);
#11943=AXIS2_PLACEMENT_3D('',#17670,#13956,#13957);
#11944=AXIS2_PLACEMENT_3D('',#17671,#13958,#13959);
#11945=AXIS2_PLACEMENT_3D('',#17679,#13964,#13965);
#11946=AXIS2_PLACEMENT_3D('',#17685,#13969,#13970);
#11947=AXIS2_PLACEMENT_3D('',#17691,#13974,#13975);
#11948=AXIS2_PLACEMENT_3D('',#17697,#13979,#13980);
#11949=AXIS2_PLACEMENT_3D('',#17703,#13984,#13985);
#11950=AXIS2_PLACEMENT_3D('',#17709,#13989,#13990);
#11951=AXIS2_PLACEMENT_3D('',#17715,#13994,#13995);
#11952=AXIS2_PLACEMENT_3D('',#17720,#13999,#14000);
#11953=AXIS2_PLACEMENT_3D('',#17724,#14003,#14004);
#11954=AXIS2_PLACEMENT_3D('',#17728,#14007,#14008);
#11955=AXIS2_PLACEMENT_3D('',#17732,#14011,#14012);
#11956=AXIS2_PLACEMENT_3D('',#17736,#14015,#14016);
#11957=AXIS2_PLACEMENT_3D('',#17740,#14019,#14020);
#11958=AXIS2_PLACEMENT_3D('',#17744,#14023,#14024);
#11959=AXIS2_PLACEMENT_3D('',#17748,#14027,#14028);
#11960=AXIS2_PLACEMENT_3D('',#17752,#14031,#14032);
#11961=AXIS2_PLACEMENT_3D('',#17756,#14035,#14036);
#11962=AXIS2_PLACEMENT_3D('',#17758,#14038,#14039);
#11963=AXIS2_PLACEMENT_3D('',#17759,#14040,#14041);
#11964=AXIS2_PLACEMENT_3D('',#17760,#14042,#14043);
#11965=AXIS2_PLACEMENT_3D('',#17761,#14044,#14045);
#11966=AXIS2_PLACEMENT_3D('',#17762,#14046,#14047);
#11967=AXIS2_PLACEMENT_3D('',#17763,#14048,#14049);
#11968=AXIS2_PLACEMENT_3D('',#17764,#14050,#14051);
#11969=AXIS2_PLACEMENT_3D('',#17765,#14052,#14053);
#11970=AXIS2_PLACEMENT_3D('',#17766,#14054,#14055);
#11971=AXIS2_PLACEMENT_3D('',#17767,#14056,#14057);
#11972=AXIS2_PLACEMENT_3D('',#17768,#14058,#14059);
#11973=AXIS2_PLACEMENT_3D('',#17769,#14060,#14061);
#11974=AXIS2_PLACEMENT_3D('',#17770,#14062,#14063);
#11975=AXIS2_PLACEMENT_3D('',#17771,#14064,#14065);
#11976=AXIS2_PLACEMENT_3D('',#17772,#14066,#14067);
#11977=AXIS2_PLACEMENT_3D('',#17773,#14068,#14069);
#11978=AXIS2_PLACEMENT_3D('',#17774,#14070,#14071);
#11979=AXIS2_PLACEMENT_3D('',#17775,#14072,#14073);
#11980=AXIS2_PLACEMENT_3D('',#17777,#14074,#14075);
#11981=AXIS2_PLACEMENT_3D('',#17779,#14077,#14078);
#11982=AXIS2_PLACEMENT_3D('',#17780,#14079,#14080);
#11983=AXIS2_PLACEMENT_3D('',#17781,#14081,#14082);
#11984=AXIS2_PLACEMENT_3D('',#17859,#14084,#14085);
#11985=AXIS2_PLACEMENT_3D('',#17861,#14086,#14087);
#11986=AXIS2_PLACEMENT_3D('',#17864,#14089,#14090);
#11987=AXIS2_PLACEMENT_3D('',#17865,#14091,#14092);
#11988=AXIS2_PLACEMENT_3D('',#17874,#14097,#14098);
#11989=AXIS2_PLACEMENT_3D('',#17880,#14102,#14103);
#11990=AXIS2_PLACEMENT_3D('',#17886,#14107,#14108);
#11991=AXIS2_PLACEMENT_3D('',#17892,#14112,#14113);
#11992=AXIS2_PLACEMENT_3D('',#17898,#14117,#14118);
#11993=AXIS2_PLACEMENT_3D('',#17904,#14122,#14123);
#11994=AXIS2_PLACEMENT_3D('',#17910,#14127,#14128);
#11995=AXIS2_PLACEMENT_3D('',#17916,#14132,#14133);
#11996=AXIS2_PLACEMENT_3D('',#17922,#14137,#14138);
#11997=AXIS2_PLACEMENT_3D('',#17928,#14142,#14143);
#11998=AXIS2_PLACEMENT_3D('',#17934,#14147,#14148);
#11999=AXIS2_PLACEMENT_3D('',#17940,#14152,#14153);
#12000=AXIS2_PLACEMENT_3D('',#17946,#14157,#14158);
#12001=AXIS2_PLACEMENT_3D('',#17952,#14162,#14163);
#12002=AXIS2_PLACEMENT_3D('',#17958,#14167,#14168);
#12003=AXIS2_PLACEMENT_3D('',#17964,#14172,#14173);
#12004=AXIS2_PLACEMENT_3D('',#17970,#14177,#14178);
#12005=AXIS2_PLACEMENT_3D('',#17973,#14181,#14182);
#12006=AXIS2_PLACEMENT_3D('',#17974,#14183,#14184);
#12007=AXIS2_PLACEMENT_3D('',#17975,#14185,#14186);
#12008=AXIS2_PLACEMENT_3D('',#17976,#14187,#14188);
#12009=AXIS2_PLACEMENT_3D('',#17977,#14189,#14190);
#12010=AXIS2_PLACEMENT_3D('',#17978,#14191,#14192);
#12011=AXIS2_PLACEMENT_3D('',#17979,#14193,#14194);
#12012=AXIS2_PLACEMENT_3D('',#17980,#14195,#14196);
#12013=AXIS2_PLACEMENT_3D('',#17981,#14197,#14198);
#12014=AXIS2_PLACEMENT_3D('',#17982,#14199,#14200);
#12015=AXIS2_PLACEMENT_3D('',#17983,#14201,#14202);
#12016=AXIS2_PLACEMENT_3D('',#17984,#14203,#14204);
#12017=AXIS2_PLACEMENT_3D('',#17985,#14205,#14206);
#12018=AXIS2_PLACEMENT_3D('',#17986,#14207,#14208);
#12019=AXIS2_PLACEMENT_3D('',#17988,#14209,#14210);
#12020=AXIS2_PLACEMENT_3D('',#17990,#14211,#14212);
#12021=AXIS2_PLACEMENT_3D('',#18012,#14223,#14224);
#12022=AXIS2_PLACEMENT_3D('',#18033,#14235,#14236);
#12023=AXIS2_PLACEMENT_3D('',#18034,#14237,#14238);
#12024=AXIS2_PLACEMENT_3D('',#18035,#14239,#14240);
#12025=AXIS2_PLACEMENT_3D('',#18036,#14241,#14242);
#12026=AXIS2_PLACEMENT_3D('',#18037,#14243,#14244);
#12027=AXIS2_PLACEMENT_3D('',#18038,#14245,#14246);
#12028=AXIS2_PLACEMENT_3D('',#18044,#14250,#14251);
#12029=AXIS2_PLACEMENT_3D('',#18048,#14254,#14255);
#12030=AXIS2_PLACEMENT_3D('',#18052,#14258,#14259);
#12031=AXIS2_PLACEMENT_3D('',#18056,#14262,#14263);
#12032=AXIS2_PLACEMENT_3D('',#18060,#14266,#14267);
#12033=AXIS2_PLACEMENT_3D('',#18064,#14270,#14271);
#12034=AXIS2_PLACEMENT_3D('',#18068,#14274,#14275);
#12035=AXIS2_PLACEMENT_3D('',#18072,#14278,#14279);
#12036=AXIS2_PLACEMENT_3D('',#18076,#14282,#14283);
#12037=AXIS2_PLACEMENT_3D('',#18082,#14287,#14288);
#12038=AXIS2_PLACEMENT_3D('',#18088,#14292,#14293);
#12039=AXIS2_PLACEMENT_3D('',#18094,#14297,#14298);
#12040=AXIS2_PLACEMENT_3D('',#18100,#14302,#14303);
#12041=AXIS2_PLACEMENT_3D('',#18106,#14307,#14308);
#12042=AXIS2_PLACEMENT_3D('',#18112,#14312,#14313);
#12043=AXIS2_PLACEMENT_3D('',#18118,#14317,#14318);
#12044=AXIS2_PLACEMENT_3D('',#18123,#14322,#14323);
#12045=AXIS2_PLACEMENT_3D('',#18125,#14325,#14326);
#12046=AXIS2_PLACEMENT_3D('',#18126,#14327,#14328);
#12047=AXIS2_PLACEMENT_3D('',#18127,#14329,#14330);
#12048=AXIS2_PLACEMENT_3D('',#18128,#14331,#14332);
#12049=AXIS2_PLACEMENT_3D('',#18129,#14333,#14334);
#12050=AXIS2_PLACEMENT_3D('',#18130,#14335,#14336);
#12051=AXIS2_PLACEMENT_3D('',#18131,#14337,#14338);
#12052=AXIS2_PLACEMENT_3D('',#18132,#14339,#14340);
#12053=AXIS2_PLACEMENT_3D('',#18133,#14341,#14342);
#12054=AXIS2_PLACEMENT_3D('',#18134,#14343,#14344);
#12055=AXIS2_PLACEMENT_3D('',#18135,#14345,#14346);
#12056=AXIS2_PLACEMENT_3D('',#18136,#14347,#14348);
#12057=AXIS2_PLACEMENT_3D('',#18137,#14349,#14350);
#12058=AXIS2_PLACEMENT_3D('',#18138,#14351,#14352);
#12059=AXIS2_PLACEMENT_3D('',#18139,#14353,#14354);
#12060=AXIS2_PLACEMENT_3D('',#18140,#14355,#14356);
#12061=AXIS2_PLACEMENT_3D('',#18141,#14357,#14358);
#12062=AXIS2_PLACEMENT_3D('',#18142,#14359,#14360);
#12063=AXIS2_PLACEMENT_3D('',#18148,#14364,#14365);
#12064=AXIS2_PLACEMENT_3D('',#18152,#14368,#14369);
#12065=AXIS2_PLACEMENT_3D('',#18156,#14372,#14373);
#12066=AXIS2_PLACEMENT_3D('',#18160,#14376,#14377);
#12067=AXIS2_PLACEMENT_3D('',#18164,#14380,#14381);
#12068=AXIS2_PLACEMENT_3D('',#18168,#14384,#14385);
#12069=AXIS2_PLACEMENT_3D('',#18172,#14388,#14389);
#12070=AXIS2_PLACEMENT_3D('',#18176,#14392,#14393);
#12071=AXIS2_PLACEMENT_3D('',#18180,#14396,#14397);
#12072=AXIS2_PLACEMENT_3D('',#18186,#14401,#14402);
#12073=AXIS2_PLACEMENT_3D('',#18192,#14406,#14407);
#12074=AXIS2_PLACEMENT_3D('',#18198,#14411,#14412);
#12075=AXIS2_PLACEMENT_3D('',#18204,#14416,#14417);
#12076=AXIS2_PLACEMENT_3D('',#18210,#14421,#14422);
#12077=AXIS2_PLACEMENT_3D('',#18216,#14426,#14427);
#12078=AXIS2_PLACEMENT_3D('',#18222,#14431,#14432);
#12079=AXIS2_PLACEMENT_3D('',#18227,#14436,#14437);
#12080=AXIS2_PLACEMENT_3D('',#18229,#14439,#14440);
#12081=AXIS2_PLACEMENT_3D('',#18230,#14441,#14442);
#12082=AXIS2_PLACEMENT_3D('',#18231,#14443,#14444);
#12083=AXIS2_PLACEMENT_3D('',#18232,#14445,#14446);
#12084=AXIS2_PLACEMENT_3D('',#18233,#14447,#14448);
#12085=AXIS2_PLACEMENT_3D('',#18234,#14449,#14450);
#12086=AXIS2_PLACEMENT_3D('',#18235,#14451,#14452);
#12087=AXIS2_PLACEMENT_3D('',#18236,#14453,#14454);
#12088=AXIS2_PLACEMENT_3D('',#18237,#14455,#14456);
#12089=AXIS2_PLACEMENT_3D('',#18238,#14457,#14458);
#12090=AXIS2_PLACEMENT_3D('',#18239,#14459,#14460);
#12091=AXIS2_PLACEMENT_3D('',#18240,#14461,#14462);
#12092=AXIS2_PLACEMENT_3D('',#18241,#14463,#14464);
#12093=AXIS2_PLACEMENT_3D('',#18242,#14465,#14466);
#12094=AXIS2_PLACEMENT_3D('',#18243,#14467,#14468);
#12095=AXIS2_PLACEMENT_3D('',#18244,#14469,#14470);
#12096=AXIS2_PLACEMENT_3D('',#18245,#14471,#14472);
#12097=AXIS2_PLACEMENT_3D('',#18246,#14473,#14474);
#12098=AXIS2_PLACEMENT_3D('',#18248,#14475,#14476);
#12099=AXIS2_PLACEMENT_3D('',#18250,#14478,#14479);
#12100=AXIS2_PLACEMENT_3D('',#18251,#14480,#14481);
#12101=AXIS2_PLACEMENT_3D('',#18252,#14482,#14483);
#12102=AXIS2_PLACEMENT_3D('',#18271,#14492,#14493);
#12103=AXIS2_PLACEMENT_3D('',#18289,#14502,#14503);
#12104=AXIS2_PLACEMENT_3D('',#18307,#14512,#14513);
#12105=AXIS2_PLACEMENT_3D('',#18325,#14522,#14523);
#12106=AXIS2_PLACEMENT_3D('',#18343,#14532,#14533);
#12107=AXIS2_PLACEMENT_3D('',#18360,#14542,#14543);
#12108=AXIS2_PLACEMENT_3D('',#18361,#14544,#14545);
#12109=AXIS2_PLACEMENT_3D('',#18365,#14547,#14548);
#12110=AXIS2_PLACEMENT_3D('',#18367,#14550,#14551);
#12111=AXIS2_PLACEMENT_3D('',#18371,#14553,#14554);
#12112=AXIS2_PLACEMENT_3D('',#18373,#14556,#14557);
#12113=AXIS2_PLACEMENT_3D('',#18377,#14559,#14560);
#12114=AXIS2_PLACEMENT_3D('',#18379,#14562,#14563);
#12115=AXIS2_PLACEMENT_3D('',#18384,#14566,#14567);
#12116=AXIS2_PLACEMENT_3D('',#18385,#14568,#14569);
#12117=AXIS2_PLACEMENT_3D('',#18390,#14572,#14573);
#12118=AXIS2_PLACEMENT_3D('',#18391,#14574,#14575);
#12119=AXIS2_PLACEMENT_3D('',#18396,#14578,#14579);
#12120=AXIS2_PLACEMENT_3D('',#18397,#14580,#14581);
#12121=AXIS2_PLACEMENT_3D('',#18488,#14630,#14631);
#12122=AXIS2_PLACEMENT_3D('',#18498,#14637,#14638);
#12123=AXIS2_PLACEMENT_3D('',#18502,#14641,#14642);
#12124=AXIS2_PLACEMENT_3D('',#18506,#14645,#14646);
#12125=AXIS2_PLACEMENT_3D('',#18510,#14649,#14650);
#12126=AXIS2_PLACEMENT_3D('',#18514,#14653,#14654);
#12127=AXIS2_PLACEMENT_3D('',#18518,#14657,#14658);
#12128=AXIS2_PLACEMENT_3D('',#18522,#14661,#14662);
#12129=AXIS2_PLACEMENT_3D('',#18526,#14665,#14666);
#12130=AXIS2_PLACEMENT_3D('',#18550,#14679,#14680);
#12131=AXIS2_PLACEMENT_3D('',#18553,#14683,#14684);
#12132=AXIS2_PLACEMENT_3D('',#18555,#14686,#14687);
#12133=AXIS2_PLACEMENT_3D('',#18557,#14689,#14690);
#12134=AXIS2_PLACEMENT_3D('',#18559,#14692,#14693);
#12135=AXIS2_PLACEMENT_3D('',#18560,#14694,#14695);
#12136=AXIS2_PLACEMENT_3D('',#18564,#14698,#14699);
#12137=AXIS2_PLACEMENT_3D('',#18568,#14702,#14703);
#12138=AXIS2_PLACEMENT_3D('',#18572,#14706,#14707);
#12139=AXIS2_PLACEMENT_3D('',#18576,#14710,#14711);
#12140=AXIS2_PLACEMENT_3D('',#18580,#14714,#14715);
#12141=AXIS2_PLACEMENT_3D('',#18584,#14718,#14719);
#12142=AXIS2_PLACEMENT_3D('',#18586,#14721,#14722);
#12143=AXIS2_PLACEMENT_3D('',#18587,#14723,#14724);
#12144=AXIS2_PLACEMENT_3D('',#18597,#14730,#14731);
#12145=AXIS2_PLACEMENT_3D('',#18601,#14734,#14735);
#12146=AXIS2_PLACEMENT_3D('',#18605,#14738,#14739);
#12147=AXIS2_PLACEMENT_3D('',#18609,#14742,#14743);
#12148=AXIS2_PLACEMENT_3D('',#18613,#14746,#14747);
#12149=AXIS2_PLACEMENT_3D('',#18617,#14750,#14751);
#12150=AXIS2_PLACEMENT_3D('',#18621,#14754,#14755);
#12151=AXIS2_PLACEMENT_3D('',#18625,#14758,#14759);
#12152=AXIS2_PLACEMENT_3D('',#18649,#14772,#14773);
#12153=AXIS2_PLACEMENT_3D('',#18652,#14776,#14777);
#12154=AXIS2_PLACEMENT_3D('',#18654,#14779,#14780);
#12155=AXIS2_PLACEMENT_3D('',#18656,#14782,#14783);
#12156=AXIS2_PLACEMENT_3D('',#18658,#14785,#14786);
#12157=AXIS2_PLACEMENT_3D('',#18659,#14787,#14788);
#12158=AXIS2_PLACEMENT_3D('',#18663,#14791,#14792);
#12159=AXIS2_PLACEMENT_3D('',#18667,#14795,#14796);
#12160=AXIS2_PLACEMENT_3D('',#18671,#14799,#14800);
#12161=AXIS2_PLACEMENT_3D('',#18675,#14803,#14804);
#12162=AXIS2_PLACEMENT_3D('',#18679,#14807,#14808);
#12163=AXIS2_PLACEMENT_3D('',#18683,#14811,#14812);
#12164=AXIS2_PLACEMENT_3D('',#18685,#14814,#14815);
#12165=AXIS2_PLACEMENT_3D('',#18686,#14816,#14817);
#12166=AXIS2_PLACEMENT_3D('',#18696,#14823,#14824);
#12167=AXIS2_PLACEMENT_3D('',#18700,#14827,#14828);
#12168=AXIS2_PLACEMENT_3D('',#18704,#14831,#14832);
#12169=AXIS2_PLACEMENT_3D('',#18708,#14835,#14836);
#12170=AXIS2_PLACEMENT_3D('',#18712,#14839,#14840);
#12171=AXIS2_PLACEMENT_3D('',#18716,#14843,#14844);
#12172=AXIS2_PLACEMENT_3D('',#18720,#14847,#14848);
#12173=AXIS2_PLACEMENT_3D('',#18724,#14851,#14852);
#12174=AXIS2_PLACEMENT_3D('',#18748,#14865,#14866);
#12175=AXIS2_PLACEMENT_3D('',#18751,#14869,#14870);
#12176=AXIS2_PLACEMENT_3D('',#18753,#14872,#14873);
#12177=AXIS2_PLACEMENT_3D('',#18755,#14875,#14876);
#12178=AXIS2_PLACEMENT_3D('',#18757,#14878,#14879);
#12179=AXIS2_PLACEMENT_3D('',#18758,#14880,#14881);
#12180=AXIS2_PLACEMENT_3D('',#18762,#14884,#14885);
#12181=AXIS2_PLACEMENT_3D('',#18766,#14888,#14889);
#12182=AXIS2_PLACEMENT_3D('',#18770,#14892,#14893);
#12183=AXIS2_PLACEMENT_3D('',#18774,#14896,#14897);
#12184=AXIS2_PLACEMENT_3D('',#18778,#14900,#14901);
#12185=AXIS2_PLACEMENT_3D('',#18782,#14904,#14905);
#12186=AXIS2_PLACEMENT_3D('',#18784,#14907,#14908);
#12187=AXIS2_PLACEMENT_3D('',#18785,#14909,#14910);
#12188=AXIS2_PLACEMENT_3D('',#18795,#14916,#14917);
#12189=AXIS2_PLACEMENT_3D('',#18799,#14920,#14921);
#12190=AXIS2_PLACEMENT_3D('',#18803,#14924,#14925);
#12191=AXIS2_PLACEMENT_3D('',#18807,#14928,#14929);
#12192=AXIS2_PLACEMENT_3D('',#18811,#14932,#14933);
#12193=AXIS2_PLACEMENT_3D('',#18815,#14936,#14937);
#12194=AXIS2_PLACEMENT_3D('',#18819,#14940,#14941);
#12195=AXIS2_PLACEMENT_3D('',#18823,#14944,#14945);
#12196=AXIS2_PLACEMENT_3D('',#18847,#14958,#14959);
#12197=AXIS2_PLACEMENT_3D('',#18850,#14962,#14963);
#12198=AXIS2_PLACEMENT_3D('',#18852,#14965,#14966);
#12199=AXIS2_PLACEMENT_3D('',#18854,#14968,#14969);
#12200=AXIS2_PLACEMENT_3D('',#18856,#14971,#14972);
#12201=AXIS2_PLACEMENT_3D('',#18857,#14973,#14974);
#12202=AXIS2_PLACEMENT_3D('',#18861,#14977,#14978);
#12203=AXIS2_PLACEMENT_3D('',#18865,#14981,#14982);
#12204=AXIS2_PLACEMENT_3D('',#18869,#14985,#14986);
#12205=AXIS2_PLACEMENT_3D('',#18873,#14989,#14990);
#12206=AXIS2_PLACEMENT_3D('',#18877,#14993,#14994);
#12207=AXIS2_PLACEMENT_3D('',#18881,#14997,#14998);
#12208=AXIS2_PLACEMENT_3D('',#18883,#15000,#15001);
#12209=AXIS2_PLACEMENT_3D('',#18884,#15002,#15003);
#12210=AXIS2_PLACEMENT_3D('',#18894,#15009,#15010);
#12211=AXIS2_PLACEMENT_3D('',#18898,#15013,#15014);
#12212=AXIS2_PLACEMENT_3D('',#18902,#15017,#15018);
#12213=AXIS2_PLACEMENT_3D('',#18906,#15021,#15022);
#12214=AXIS2_PLACEMENT_3D('',#18910,#15025,#15026);
#12215=AXIS2_PLACEMENT_3D('',#18914,#15029,#15030);
#12216=AXIS2_PLACEMENT_3D('',#18918,#15033,#15034);
#12217=AXIS2_PLACEMENT_3D('',#18922,#15037,#15038);
#12218=AXIS2_PLACEMENT_3D('',#18946,#15051,#15052);
#12219=AXIS2_PLACEMENT_3D('',#18949,#15055,#15056);
#12220=AXIS2_PLACEMENT_3D('',#18951,#15058,#15059);
#12221=AXIS2_PLACEMENT_3D('',#18953,#15061,#15062);
#12222=AXIS2_PLACEMENT_3D('',#18955,#15064,#15065);
#12223=AXIS2_PLACEMENT_3D('',#18956,#15066,#15067);
#12224=AXIS2_PLACEMENT_3D('',#18960,#15070,#15071);
#12225=AXIS2_PLACEMENT_3D('',#18964,#15074,#15075);
#12226=AXIS2_PLACEMENT_3D('',#18968,#15078,#15079);
#12227=AXIS2_PLACEMENT_3D('',#18972,#15082,#15083);
#12228=AXIS2_PLACEMENT_3D('',#18976,#15086,#15087);
#12229=AXIS2_PLACEMENT_3D('',#18980,#15090,#15091);
#12230=AXIS2_PLACEMENT_3D('',#18982,#15093,#15094);
#12231=AXIS2_PLACEMENT_3D('',#18983,#15095,#15096);
#12232=AXIS2_PLACEMENT_3D('',#18993,#15102,#15103);
#12233=AXIS2_PLACEMENT_3D('',#18997,#15106,#15107);
#12234=AXIS2_PLACEMENT_3D('',#19001,#15110,#15111);
#12235=AXIS2_PLACEMENT_3D('',#19005,#15114,#15115);
#12236=AXIS2_PLACEMENT_3D('',#19009,#15118,#15119);
#12237=AXIS2_PLACEMENT_3D('',#19013,#15122,#15123);
#12238=AXIS2_PLACEMENT_3D('',#19017,#15126,#15127);
#12239=AXIS2_PLACEMENT_3D('',#19021,#15130,#15131);
#12240=AXIS2_PLACEMENT_3D('',#19045,#15144,#15145);
#12241=AXIS2_PLACEMENT_3D('',#19048,#15148,#15149);
#12242=AXIS2_PLACEMENT_3D('',#19050,#15151,#15152);
#12243=AXIS2_PLACEMENT_3D('',#19052,#15154,#15155);
#12244=AXIS2_PLACEMENT_3D('',#19054,#15157,#15158);
#12245=AXIS2_PLACEMENT_3D('',#19055,#15159,#15160);
#12246=AXIS2_PLACEMENT_3D('',#19059,#15163,#15164);
#12247=AXIS2_PLACEMENT_3D('',#19063,#15167,#15168);
#12248=AXIS2_PLACEMENT_3D('',#19067,#15171,#15172);
#12249=AXIS2_PLACEMENT_3D('',#19071,#15175,#15176);
#12250=AXIS2_PLACEMENT_3D('',#19075,#15179,#15180);
#12251=AXIS2_PLACEMENT_3D('',#19079,#15183,#15184);
#12252=AXIS2_PLACEMENT_3D('',#19081,#15186,#15187);
#12253=AXIS2_PLACEMENT_3D('',#19082,#15188,#15189);
#12254=AXIS2_PLACEMENT_3D('',#19083,#15190,#15191);
#12255=AXIS2_PLACEMENT_3D('',#19084,#15192,#15193);
#12256=AXIS2_PLACEMENT_3D('',#19085,#15194,#15195);
#12257=AXIS2_PLACEMENT_3D('',#19086,#15196,#15197);
#12258=AXIS2_PLACEMENT_3D('',#19095,#15202,#15203);
#12259=AXIS2_PLACEMENT_3D('',#19099,#15205,#15206);
#12260=AXIS2_PLACEMENT_3D('',#19100,#15207,#15208);
#12261=AXIS2_PLACEMENT_3D('',#19101,#15209,#15210);
#12262=AXIS2_PLACEMENT_3D('',#19107,#15214,#15215);
#12263=AXIS2_PLACEMENT_3D('',#19108,#15216,#15217);
#12264=AXIS2_PLACEMENT_3D('',#19109,#15218,#15219);
#12265=AXIS2_PLACEMENT_3D('',#19110,#15220,#15221);
#12266=AXIS2_PLACEMENT_3D('',#19114,#15223,#15224);
#12267=AXIS2_PLACEMENT_3D('',#19116,#15226,#15227);
#12268=AXIS2_PLACEMENT_3D('',#19120,#15230,#15231);
#12269=AXIS2_PLACEMENT_3D('',#19121,#15232,#15233);
#12270=AXIS2_PLACEMENT_3D('',#19127,#15237,#15238);
#12271=AXIS2_PLACEMENT_3D('',#19130,#15240,#15241);
#12272=AXIS2_PLACEMENT_3D('',#19131,#15242,#15243);
#12273=AXIS2_PLACEMENT_3D('',#19137,#15247,#15248);
#12274=AXIS2_PLACEMENT_3D('',#19138,#15249,#15250);
#12275=AXIS2_PLACEMENT_3D('',#19139,#15251,#15252);
#12276=AXIS2_PLACEMENT_3D('',#19140,#15253,#15254);
#12277=AXIS2_PLACEMENT_3D('',#19142,#15256,#15257);
#12278=AXIS2_PLACEMENT_3D('',#19143,#15258,#15259);
#12279=AXIS2_PLACEMENT_3D('',#19144,#15260,#15261);
#12280=AXIS2_PLACEMENT_3D('',#19145,#15262,#15263);
#12281=AXIS2_PLACEMENT_3D('',#19154,#15268,#15269);
#12282=AXIS2_PLACEMENT_3D('',#19160,#15273,#15274);
#12283=AXIS2_PLACEMENT_3D('',#19166,#15278,#15279);
#12284=AXIS2_PLACEMENT_3D('',#19172,#15283,#15284);
#12285=AXIS2_PLACEMENT_3D('',#19178,#15288,#15289);
#12286=AXIS2_PLACEMENT_3D('',#19181,#15292,#15293);
#12287=AXIS2_PLACEMENT_3D('',#19182,#15294,#15295);
#12288=AXIS2_PLACEMENT_3D('',#19184,#15296,#15297);
#12289=AXIS2_PLACEMENT_3D('',#19185,#15298,#15299);
#12290=AXIS2_PLACEMENT_3D('',#19187,#15300,#15301);
#12291=AXIS2_PLACEMENT_3D('',#19189,#15303,#15304);
#12292=AXIS2_PLACEMENT_3D('',#19191,#15305,#15306);
#12293=AXIS2_PLACEMENT_3D('',#19193,#15308,#15309);
#12294=AXIS2_PLACEMENT_3D('',#19195,#15310,#15311);
#12295=AXIS2_PLACEMENT_3D('',#19197,#15313,#15314);
#12296=AXIS2_PLACEMENT_3D('',#19198,#15315,#15316);
#12297=AXIS2_PLACEMENT_3D('',#19199,#15317,#15318);
#12298=AXIS2_PLACEMENT_3D('',#19201,#15319,#15320);
#12299=AXIS2_PLACEMENT_3D('',#19202,#15321,#15322);
#12300=AXIS2_PLACEMENT_3D('',#19204,#15323,#15324);
#12301=AXIS2_PLACEMENT_3D('',#19206,#15326,#15327);
#12302=AXIS2_PLACEMENT_3D('',#19208,#15328,#15329);
#12303=AXIS2_PLACEMENT_3D('',#19210,#15331,#15332);
#12304=AXIS2_PLACEMENT_3D('',#19212,#15333,#15334);
#12305=AXIS2_PLACEMENT_3D('',#19214,#15336,#15337);
#12306=AXIS2_PLACEMENT_3D('',#19216,#15338,#15339);
#12307=AXIS2_PLACEMENT_3D('',#19217,#15340,#15341);
#12308=AXIS2_PLACEMENT_3D('',#19219,#15342,#15343);
#12309=AXIS2_PLACEMENT_3D('',#19221,#15345,#15346);
#12310=AXIS2_PLACEMENT_3D('',#19223,#15347,#15348);
#12311=AXIS2_PLACEMENT_3D('',#19225,#15350,#15351);
#12312=AXIS2_PLACEMENT_3D('',#19227,#15352,#15353);
#12313=AXIS2_PLACEMENT_3D('',#19229,#15355,#15356);
#12314=AXIS2_PLACEMENT_3D('',#19230,#15357,#15358);
#12315=AXIS2_PLACEMENT_3D('',#19239,#15363,#15364);
#12316=AXIS2_PLACEMENT_3D('',#19245,#15368,#15369);
#12317=AXIS2_PLACEMENT_3D('',#19251,#15373,#15374);
#12318=AXIS2_PLACEMENT_3D('',#19257,#15378,#15379);
#12319=AXIS2_PLACEMENT_3D('',#19263,#15383,#15384);
#12320=AXIS2_PLACEMENT_3D('',#19266,#15387,#15388);
#12321=AXIS2_PLACEMENT_3D('',#19267,#15389,#15390);
#12322=AXIS2_PLACEMENT_3D('',#19268,#15391,#15392);
#12323=AXIS2_PLACEMENT_3D('',#19269,#15393,#15394);
#12324=AXIS2_PLACEMENT_3D('',#19270,#15395,#15396);
#12325=AXIS2_PLACEMENT_3D('',#19271,#15397,#15398);
#12326=AXIS2_PLACEMENT_3D('',#19272,#15399,#15400);
#12327=AXIS2_PLACEMENT_3D('',#19273,#15401,#15402);
#12328=AXIS2_PLACEMENT_3D('',#19274,#15403,#15404);
#12329=AXIS2_PLACEMENT_3D('',#19275,#15405,#15406);
#12330=AXIS2_PLACEMENT_3D('',#19276,#15407,#15408);
#12331=AXIS2_PLACEMENT_3D('',#19277,#15409,#15410);
#12332=AXIS2_PLACEMENT_3D('',#19278,#15411,#15412);
#12333=AXIS2_PLACEMENT_3D('',#19279,#15413,#15414);
#12334=AXIS2_PLACEMENT_3D('',#19280,#15415,#15416);
#12335=AXIS2_PLACEMENT_3D('',#19281,#15417,#15418);
#12336=AXIS2_PLACEMENT_3D('',#19282,#15419,#15420);
#12337=AXIS2_PLACEMENT_3D('',#19283,#15421,#15422);
#12338=AXIS2_PLACEMENT_3D('',#19284,#15423,#15424);
#12339=AXIS2_PLACEMENT_3D('',#19285,#15425,#15426);
#12340=DIRECTION('axis',(0.,0.,1.));
#12341=DIRECTION('refdir',(1.,0.,0.));
#12342=DIRECTION('axis',(0.,0.,1.));
#12343=DIRECTION('refdir',(1.,0.,0.));
#12344=DIRECTION('axis',(0.,0.,1.));
#12345=DIRECTION('refdir',(1.,0.,0.));
#12346=DIRECTION('center_axis',(0.,0.,1.));
#12347=DIRECTION('ref_axis',(1.,0.,0.));
#12348=DIRECTION('center_axis',(0.,0.,1.));
#12349=DIRECTION('ref_axis',(1.,0.,0.));
#12350=DIRECTION('',(0.,0.,1.));
#12351=DIRECTION('center_axis',(0.,0.,-1.));
#12352=DIRECTION('ref_axis',(1.,0.,0.));
#12353=DIRECTION('center_axis',(0.,0.,1.));
#12354=DIRECTION('ref_axis',(1.,0.,0.));
#12355=DIRECTION('center_axis',(0.,0.,1.));
#12356=DIRECTION('ref_axis',(1.,0.,0.));
#12357=DIRECTION('',(0.,0.,1.));
#12358=DIRECTION('center_axis',(0.,0.,-1.));
#12359=DIRECTION('ref_axis',(1.,0.,0.));
#12360=DIRECTION('center_axis',(0.,0.,1.));
#12361=DIRECTION('ref_axis',(1.,0.,0.));
#12362=DIRECTION('center_axis',(0.,0.,1.));
#12363=DIRECTION('ref_axis',(1.,0.,0.));
#12364=DIRECTION('',(0.,0.,1.));
#12365=DIRECTION('center_axis',(0.,0.,-1.));
#12366=DIRECTION('ref_axis',(1.,0.,0.));
#12367=DIRECTION('center_axis',(0.,0.,1.));
#12368=DIRECTION('ref_axis',(1.,0.,0.));
#12369=DIRECTION('center_axis',(0.,0.,1.));
#12370=DIRECTION('ref_axis',(1.,0.,0.));
#12371=DIRECTION('',(0.,0.,1.));
#12372=DIRECTION('center_axis',(0.,0.,-1.));
#12373=DIRECTION('ref_axis',(1.,0.,0.));
#12374=DIRECTION('center_axis',(0.,0.,1.));
#12375=DIRECTION('ref_axis',(1.,0.,0.));
#12376=DIRECTION('center_axis',(0.,0.,1.));
#12377=DIRECTION('ref_axis',(1.,0.,0.));
#12378=DIRECTION('',(0.,0.,1.));
#12379=DIRECTION('center_axis',(0.,0.,-1.));
#12380=DIRECTION('ref_axis',(1.,0.,0.));
#12381=DIRECTION('center_axis',(0.,0.,1.));
#12382=DIRECTION('ref_axis',(1.,0.,0.));
#12383=DIRECTION('center_axis',(0.,0.,1.));
#12384=DIRECTION('ref_axis',(1.,0.,0.));
#12385=DIRECTION('',(0.,0.,1.));
#12386=DIRECTION('center_axis',(0.,0.,-1.));
#12387=DIRECTION('ref_axis',(1.,0.,0.));
#12388=DIRECTION('center_axis',(0.,1.,0.));
#12389=DIRECTION('ref_axis',(-1.,0.,0.));
#12390=DIRECTION('',(-1.,0.,0.));
#12391=DIRECTION('',(0.,0.,1.));
#12392=DIRECTION('',(-1.,0.,0.));
#12393=DIRECTION('',(0.,0.,1.));
#12394=DIRECTION('center_axis',(1.,0.,0.));
#12395=DIRECTION('ref_axis',(0.,1.,0.));
#12396=DIRECTION('',(0.,1.,0.));
#12397=DIRECTION('',(0.,1.,0.));
#12398=DIRECTION('',(0.,0.,1.));
#12399=DIRECTION('center_axis',(0.,-1.,0.));
#12400=DIRECTION('ref_axis',(1.,0.,0.));
#12401=DIRECTION('',(1.,0.,0.));
#12402=DIRECTION('',(1.,0.,0.));
#12403=DIRECTION('',(0.,0.,1.));
#12404=DIRECTION('center_axis',(-1.,0.,0.));
#12405=DIRECTION('ref_axis',(0.,-1.,0.));
#12406=DIRECTION('',(0.,-1.,0.));
#12407=DIRECTION('',(0.,-1.,0.));
#12408=DIRECTION('center_axis',(0.,0.,1.));
#12409=DIRECTION('ref_axis',(1.,0.,0.));
#12410=DIRECTION('center_axis',(0.,0.,1.));
#12411=DIRECTION('ref_axis',(1.,0.,0.));
#12412=DIRECTION('axis',(0.,0.,1.));
#12413=DIRECTION('refdir',(1.,0.,0.));
#12414=DIRECTION('center_axis',(0.,1.,0.));
#12415=DIRECTION('ref_axis',(-1.,0.,0.));
#12416=DIRECTION('',(-1.,0.,0.));
#12417=DIRECTION('',(0.,0.,1.));
#12418=DIRECTION('',(-1.,0.,0.));
#12419=DIRECTION('',(0.,0.,1.));
#12420=DIRECTION('center_axis',(1.,0.,0.));
#12421=DIRECTION('ref_axis',(0.,1.,0.));
#12422=DIRECTION('',(0.,1.,0.));
#12423=DIRECTION('',(0.,1.,0.));
#12424=DIRECTION('',(0.,0.,1.));
#12425=DIRECTION('center_axis',(0.,-1.,0.));
#12426=DIRECTION('ref_axis',(1.,0.,0.));
#12427=DIRECTION('',(1.,0.,0.));
#12428=DIRECTION('',(1.,0.,0.));
#12429=DIRECTION('',(0.,0.,1.));
#12430=DIRECTION('center_axis',(-1.,0.,0.));
#12431=DIRECTION('ref_axis',(0.,-1.,0.));
#12432=DIRECTION('',(0.,-1.,0.));
#12433=DIRECTION('',(0.,-1.,0.));
#12434=DIRECTION('center_axis',(0.,0.,1.));
#12435=DIRECTION('ref_axis',(1.,0.,0.));
#12436=DIRECTION('center_axis',(0.,0.,1.));
#12437=DIRECTION('ref_axis',(1.,0.,0.));
#12438=DIRECTION('axis',(0.,0.,1.));
#12439=DIRECTION('refdir',(1.,0.,0.));
#12440=DIRECTION('center_axis',(0.,1.,0.));
#12441=DIRECTION('ref_axis',(-1.,0.,0.));
#12442=DIRECTION('',(-1.,0.,0.));
#12443=DIRECTION('',(0.,0.,1.));
#12444=DIRECTION('',(-1.,0.,0.));
#12445=DIRECTION('',(0.,0.,1.));
#12446=DIRECTION('center_axis',(1.,0.,0.));
#12447=DIRECTION('ref_axis',(0.,1.,0.));
#12448=DIRECTION('',(0.,1.,0.));
#12449=DIRECTION('',(0.,1.,0.));
#12450=DIRECTION('',(0.,0.,1.));
#12451=DIRECTION('center_axis',(0.,-1.,0.));
#12452=DIRECTION('ref_axis',(1.,0.,0.));
#12453=DIRECTION('',(1.,0.,0.));
#12454=DIRECTION('',(1.,0.,0.));
#12455=DIRECTION('',(0.,0.,1.));
#12456=DIRECTION('center_axis',(-1.,0.,0.));
#12457=DIRECTION('ref_axis',(0.,-1.,0.));
#12458=DIRECTION('',(0.,-1.,0.));
#12459=DIRECTION('',(0.,-1.,0.));
#12460=DIRECTION('center_axis',(0.,0.,1.));
#12461=DIRECTION('ref_axis',(1.,0.,0.));
#12462=DIRECTION('center_axis',(0.,0.,1.));
#12463=DIRECTION('ref_axis',(1.,0.,0.));
#12464=DIRECTION('axis',(0.,0.,1.));
#12465=DIRECTION('refdir',(1.,0.,0.));
#12466=DIRECTION('center_axis',(0.,0.,1.));
#12467=DIRECTION('ref_axis',(1.,0.,0.));
#12468=DIRECTION('center_axis',(0.,0.,-1.));
#12469=DIRECTION('ref_axis',(1.,0.,0.));
#12470=DIRECTION('',(0.,0.,-1.));
#12471=DIRECTION('center_axis',(0.,0.,-1.));
#12472=DIRECTION('ref_axis',(1.,0.,0.));
#12473=DIRECTION('center_axis',(0.,0.,1.));
#12474=DIRECTION('ref_axis',(1.,0.,0.));
#12475=DIRECTION('center_axis',(0.,0.,1.));
#12476=DIRECTION('ref_axis',(1.,0.,0.));
#12477=DIRECTION('',(0.,0.,-1.));
#12478=DIRECTION('center_axis',(0.,0.,1.));
#12479=DIRECTION('ref_axis',(1.,0.,0.));
#12480=DIRECTION('center_axis',(0.,0.,1.));
#12481=DIRECTION('ref_axis',(1.,0.,0.));
#12482=DIRECTION('center_axis',(0.,0.,1.));
#12483=DIRECTION('ref_axis',(1.,0.,0.));
#12484=DIRECTION('axis',(0.,0.,1.));
#12485=DIRECTION('refdir',(1.,0.,0.));
#12486=DIRECTION('center_axis',(0.,0.,1.));
#12487=DIRECTION('ref_axis',(1.,0.,0.));
#12488=DIRECTION('center_axis',(0.,0.,-1.));
#12489=DIRECTION('ref_axis',(1.,0.,0.));
#12490=DIRECTION('',(0.,0.,-1.));
#12491=DIRECTION('center_axis',(0.,0.,-1.));
#12492=DIRECTION('ref_axis',(1.,0.,0.));
#12493=DIRECTION('center_axis',(0.,0.,1.));
#12494=DIRECTION('ref_axis',(1.,0.,0.));
#12495=DIRECTION('center_axis',(0.,0.,1.));
#12496=DIRECTION('ref_axis',(1.,0.,0.));
#12497=DIRECTION('',(0.,0.,-1.));
#12498=DIRECTION('center_axis',(0.,0.,1.));
#12499=DIRECTION('ref_axis',(1.,0.,0.));
#12500=DIRECTION('center_axis',(0.,0.,1.));
#12501=DIRECTION('ref_axis',(1.,0.,0.));
#12502=DIRECTION('center_axis',(0.,0.,1.));
#12503=DIRECTION('ref_axis',(1.,0.,0.));
#12504=DIRECTION('axis',(0.,0.,1.));
#12505=DIRECTION('refdir',(1.,0.,0.));
#12506=DIRECTION('center_axis',(0.,0.,1.));
#12507=DIRECTION('ref_axis',(1.,0.,0.));
#12508=DIRECTION('center_axis',(0.,0.,-1.));
#12509=DIRECTION('ref_axis',(1.,0.,0.));
#12510=DIRECTION('',(0.,0.,-1.));
#12511=DIRECTION('center_axis',(0.,0.,-1.));
#12512=DIRECTION('ref_axis',(1.,0.,0.));
#12513=DIRECTION('center_axis',(0.,0.,1.));
#12514=DIRECTION('ref_axis',(1.,0.,0.));
#12515=DIRECTION('center_axis',(0.,0.,1.));
#12516=DIRECTION('ref_axis',(1.,0.,0.));
#12517=DIRECTION('',(0.,0.,-1.));
#12518=DIRECTION('center_axis',(0.,0.,1.));
#12519=DIRECTION('ref_axis',(1.,0.,0.));
#12520=DIRECTION('center_axis',(0.,0.,1.));
#12521=DIRECTION('ref_axis',(1.,0.,0.));
#12522=DIRECTION('center_axis',(0.,0.,1.));
#12523=DIRECTION('ref_axis',(1.,0.,0.));
#12524=DIRECTION('axis',(0.,0.,1.));
#12525=DIRECTION('refdir',(1.,0.,0.));
#12526=DIRECTION('center_axis',(0.,0.,1.));
#12527=DIRECTION('ref_axis',(1.,0.,0.));
#12528=DIRECTION('center_axis',(0.,0.,-1.));
#12529=DIRECTION('ref_axis',(1.,0.,0.));
#12530=DIRECTION('',(0.,0.,-1.));
#12531=DIRECTION('center_axis',(0.,0.,-1.));
#12532=DIRECTION('ref_axis',(1.,0.,0.));
#12533=DIRECTION('center_axis',(0.,0.,1.));
#12534=DIRECTION('ref_axis',(1.,0.,0.));
#12535=DIRECTION('center_axis',(0.,0.,1.));
#12536=DIRECTION('ref_axis',(1.,0.,0.));
#12537=DIRECTION('',(0.,0.,-1.));
#12538=DIRECTION('center_axis',(0.,0.,1.));
#12539=DIRECTION('ref_axis',(1.,0.,0.));
#12540=DIRECTION('center_axis',(0.,0.,1.));
#12541=DIRECTION('ref_axis',(1.,0.,0.));
#12542=DIRECTION('center_axis',(0.,0.,1.));
#12543=DIRECTION('ref_axis',(1.,0.,0.));
#12544=DIRECTION('axis',(0.,0.,1.));
#12545=DIRECTION('refdir',(1.,0.,0.));
#12546=DIRECTION('center_axis',(0.,1.,0.));
#12547=DIRECTION('ref_axis',(1.,0.,0.));
#12548=DIRECTION('center_axis',(0.,1.,0.));
#12549=DIRECTION('ref_axis',(1.,0.,0.));
#12550=DIRECTION('',(0.,1.,0.));
#12551=DIRECTION('center_axis',(0.,-1.,0.));
#12552=DIRECTION('ref_axis',(1.,0.,0.));
#12553=DIRECTION('center_axis',(0.,1.,0.));
#12554=DIRECTION('ref_axis',(1.,0.,0.));
#12555=DIRECTION('center_axis',(0.,1.,0.));
#12556=DIRECTION('ref_axis',(1.,0.,0.));
#12557=DIRECTION('',(0.,1.,0.));
#12558=DIRECTION('center_axis',(0.,-1.,0.));
#12559=DIRECTION('ref_axis',(1.,0.,0.));
#12560=DIRECTION('center_axis',(0.,1.,0.));
#12561=DIRECTION('ref_axis',(1.,0.,0.));
#12562=DIRECTION('center_axis',(0.,1.,0.));
#12563=DIRECTION('ref_axis',(1.,0.,0.));
#12564=DIRECTION('',(0.,1.,0.));
#12565=DIRECTION('center_axis',(0.,-1.,0.));
#12566=DIRECTION('ref_axis',(1.,0.,0.));
#12567=DIRECTION('center_axis',(0.,1.,0.));
#12568=DIRECTION('ref_axis',(1.,0.,0.));
#12569=DIRECTION('center_axis',(0.,1.,0.));
#12570=DIRECTION('ref_axis',(1.,0.,0.));
#12571=DIRECTION('',(0.,1.,0.));
#12572=DIRECTION('center_axis',(0.,-1.,0.));
#12573=DIRECTION('ref_axis',(1.,0.,0.));
#12574=DIRECTION('center_axis',(0.,1.,0.));
#12575=DIRECTION('ref_axis',(1.,0.,0.));
#12576=DIRECTION('center_axis',(0.,1.,0.));
#12577=DIRECTION('ref_axis',(1.,0.,0.));
#12578=DIRECTION('',(0.,1.,0.));
#12579=DIRECTION('center_axis',(0.,-1.,0.));
#12580=DIRECTION('ref_axis',(1.,0.,0.));
#12581=DIRECTION('center_axis',(0.,0.,1.));
#12582=DIRECTION('ref_axis',(1.,0.,0.));
#12583=DIRECTION('center_axis',(0.,0.,1.));
#12584=DIRECTION('ref_axis',(1.,0.,0.));
#12585=DIRECTION('',(0.,0.,1.));
#12586=DIRECTION('center_axis',(0.,0.,-1.));
#12587=DIRECTION('ref_axis',(1.,0.,0.));
#12588=DIRECTION('center_axis',(0.,0.,1.));
#12589=DIRECTION('ref_axis',(1.,0.,0.));
#12590=DIRECTION('center_axis',(0.,0.,1.));
#12591=DIRECTION('ref_axis',(1.,0.,0.));
#12592=DIRECTION('',(0.,0.,1.));
#12593=DIRECTION('center_axis',(0.,0.,-1.));
#12594=DIRECTION('ref_axis',(1.,0.,0.));
#12595=DIRECTION('center_axis',(0.,0.,1.));
#12596=DIRECTION('ref_axis',(1.,0.,0.));
#12597=DIRECTION('',(1.,0.,0.));
#12598=DIRECTION('',(0.,1.,0.));
#12599=DIRECTION('',(-1.,0.,0.));
#12600=DIRECTION('',(0.,1.,0.));
#12601=DIRECTION('center_axis',(0.,1.,0.));
#12602=DIRECTION('ref_axis',(1.,0.,0.));
#12603=DIRECTION('',(0.,0.,-1.));
#12604=DIRECTION('',(1.,0.,0.));
#12605=DIRECTION('',(0.,0.,1.));
#12606=DIRECTION('center_axis',(0.,1.,0.));
#12607=DIRECTION('ref_axis',(-1.,0.,0.));
#12608=DIRECTION('',(0.,0.,1.));
#12609=DIRECTION('',(-1.,0.,0.));
#12610=DIRECTION('',(0.,0.,1.));
#12611=DIRECTION('',(-1.,0.,0.));
#12612=DIRECTION('center_axis',(-1.,0.,0.));
#12613=DIRECTION('ref_axis',(0.,-1.,0.));
#12614=DIRECTION('',(0.,0.,1.));
#12615=DIRECTION('',(0.,-1.,0.));
#12616=DIRECTION('',(0.,-1.,0.));
#12617=DIRECTION('center_axis',(1.,0.,0.));
#12618=DIRECTION('ref_axis',(0.,1.,0.));
#12619=DIRECTION('',(0.,1.,0.));
#12620=DIRECTION('',(0.,0.,1.));
#12621=DIRECTION('',(0.,1.,0.));
#12622=DIRECTION('center_axis',(0.,-1.,0.));
#12623=DIRECTION('ref_axis',(1.,0.,0.));
#12624=DIRECTION('',(1.,0.,0.));
#12625=DIRECTION('center_axis',(0.,0.,1.));
#12626=DIRECTION('ref_axis',(1.,0.,0.));
#12627=DIRECTION('center_axis',(0.,0.,1.));
#12628=DIRECTION('ref_axis',(1.,0.,0.));
#12629=DIRECTION('axis',(0.,0.,1.));
#12630=DIRECTION('refdir',(1.,0.,0.));
#12631=DIRECTION('center_axis',(0.,1.,0.));
#12632=DIRECTION('ref_axis',(1.,0.,0.));
#12633=DIRECTION('center_axis',(0.,1.,0.));
#12634=DIRECTION('ref_axis',(1.,0.,0.));
#12635=DIRECTION('',(0.,1.,0.));
#12636=DIRECTION('center_axis',(0.,-1.,0.));
#12637=DIRECTION('ref_axis',(1.,0.,0.));
#12638=DIRECTION('center_axis',(0.,1.,0.));
#12639=DIRECTION('ref_axis',(1.,0.,0.));
#12640=DIRECTION('center_axis',(0.,1.,0.));
#12641=DIRECTION('ref_axis',(1.,0.,0.));
#12642=DIRECTION('center_axis',(0.,1.,0.));
#12643=DIRECTION('ref_axis',(1.,0.,0.));
#12644=DIRECTION('',(0.,1.,0.));
#12645=DIRECTION('center_axis',(0.,-1.,0.));
#12646=DIRECTION('ref_axis',(1.,0.,0.));
#12647=DIRECTION('center_axis',(0.,1.,0.));
#12648=DIRECTION('ref_axis',(1.,0.,0.));
#12649=DIRECTION('center_axis',(0.,1.,0.));
#12650=DIRECTION('ref_axis',(1.,0.,0.));
#12651=DIRECTION('center_axis',(0.,1.,0.));
#12652=DIRECTION('ref_axis',(1.,0.,0.));
#12653=DIRECTION('',(0.,1.,0.));
#12654=DIRECTION('center_axis',(0.,-1.,0.));
#12655=DIRECTION('ref_axis',(1.,0.,0.));
#12656=DIRECTION('center_axis',(0.,1.,0.));
#12657=DIRECTION('ref_axis',(1.,0.,0.));
#12658=DIRECTION('center_axis',(0.,1.,0.));
#12659=DIRECTION('ref_axis',(1.,0.,0.));
#12660=DIRECTION('center_axis',(0.,1.,0.));
#12661=DIRECTION('ref_axis',(1.,0.,0.));
#12662=DIRECTION('',(0.,1.,0.));
#12663=DIRECTION('center_axis',(0.,-1.,0.));
#12664=DIRECTION('ref_axis',(1.,0.,0.));
#12665=DIRECTION('center_axis',(0.,1.,0.));
#12666=DIRECTION('ref_axis',(1.,0.,0.));
#12667=DIRECTION('center_axis',(0.,1.,0.));
#12668=DIRECTION('ref_axis',(1.,0.,0.));
#12669=DIRECTION('center_axis',(0.,1.,0.));
#12670=DIRECTION('ref_axis',(1.,0.,0.));
#12671=DIRECTION('',(0.,-1.,0.));
#12672=DIRECTION('center_axis',(0.,-1.,0.));
#12673=DIRECTION('ref_axis',(1.,0.,0.));
#12674=DIRECTION('center_axis',(0.,1.,0.));
#12675=DIRECTION('ref_axis',(1.,0.,0.));
#12676=DIRECTION('center_axis',(0.,-1.,0.));
#12677=DIRECTION('ref_axis',(1.,0.,0.));
#12678=DIRECTION('center_axis',(0.,1.,0.));
#12679=DIRECTION('ref_axis',(1.,0.,0.));
#12680=DIRECTION('center_axis',(0.,1.,0.));
#12681=DIRECTION('ref_axis',(1.,0.,0.));
#12682=DIRECTION('',(0.,1.,0.));
#12683=DIRECTION('center_axis',(0.,1.,0.));
#12684=DIRECTION('ref_axis',(-1.,0.,0.));
#12685=DIRECTION('',(-1.,0.,0.));
#12686=DIRECTION('',(0.,0.,1.));
#12687=DIRECTION('',(-1.,0.,0.));
#12688=DIRECTION('',(0.,0.,1.));
#12689=DIRECTION('center_axis',(1.,0.,0.));
#12690=DIRECTION('ref_axis',(0.,1.,0.));
#12691=DIRECTION('',(0.,1.,0.));
#12692=DIRECTION('',(0.,1.,0.));
#12693=DIRECTION('',(0.,0.,1.));
#12694=DIRECTION('center_axis',(0.,-1.,0.));
#12695=DIRECTION('ref_axis',(1.,0.,0.));
#12696=DIRECTION('',(1.,0.,0.));
#12697=DIRECTION('',(1.,0.,0.));
#12698=DIRECTION('',(0.,0.,1.));
#12699=DIRECTION('center_axis',(-1.,0.,0.));
#12700=DIRECTION('ref_axis',(0.,-1.,0.));
#12701=DIRECTION('',(0.,-1.,0.));
#12702=DIRECTION('',(0.,-1.,0.));
#12703=DIRECTION('center_axis',(0.,0.,1.));
#12704=DIRECTION('ref_axis',(1.,0.,0.));
#12705=DIRECTION('center_axis',(0.,0.,1.));
#12706=DIRECTION('ref_axis',(1.,0.,0.));
#12707=DIRECTION('axis',(0.,0.,1.));
#12708=DIRECTION('refdir',(1.,0.,0.));
#12709=DIRECTION('center_axis',(-0.866025403784438,0.,0.5));
#12710=DIRECTION('ref_axis',(0.5,0.,0.866025403784438));
#12711=DIRECTION('',(-0.5,0.,-0.866025403784438));
#12712=DIRECTION('',(0.,1.,0.));
#12713=DIRECTION('',(-0.5,0.,-0.866025403784438));
#12714=DIRECTION('',(0.,1.,0.));
#12715=DIRECTION('center_axis',(-0.866025403784438,0.,-0.5));
#12716=DIRECTION('ref_axis',(-0.5,0.,0.866025403784438));
#12717=DIRECTION('',(0.5,0.,-0.866025403784438));
#12718=DIRECTION('',(0.5,0.,-0.866025403784438));
#12719=DIRECTION('',(0.,1.,0.));
#12720=DIRECTION('center_axis',(0.,0.,-1.));
#12721=DIRECTION('ref_axis',(-1.,0.,0.));
#12722=DIRECTION('',(1.,0.,0.));
#12723=DIRECTION('',(1.,0.,0.));
#12724=DIRECTION('',(0.,1.,0.));
#12725=DIRECTION('center_axis',(0.866025403784439,0.,-0.499999999999999));
#12726=DIRECTION('ref_axis',(-0.499999999999999,0.,-0.866025403784439));
#12727=DIRECTION('',(0.499999999999999,0.,0.866025403784439));
#12728=DIRECTION('',(0.499999999999999,0.,0.866025403784439));
#12729=DIRECTION('',(0.,1.,0.));
#12730=DIRECTION('center_axis',(0.866025403784439,0.,0.499999999999999));
#12731=DIRECTION('ref_axis',(0.499999999999999,0.,-0.866025403784439));
#12732=DIRECTION('',(-0.499999999999999,0.,0.866025403784439));
#12733=DIRECTION('',(-0.499999999999999,0.,0.866025403784439));
#12734=DIRECTION('',(0.,1.,0.));
#12735=DIRECTION('center_axis',(0.,0.,1.));
#12736=DIRECTION('ref_axis',(1.,0.,0.));
#12737=DIRECTION('',(-1.,0.,0.));
#12738=DIRECTION('',(-1.,0.,0.));
#12739=DIRECTION('center_axis',(0.,1.,0.));
#12740=DIRECTION('ref_axis',(1.,0.,0.));
#12741=DIRECTION('center_axis',(0.,1.,0.));
#12742=DIRECTION('ref_axis',(1.,0.,0.));
#12743=DIRECTION('center_axis',(0.,1.,0.));
#12744=DIRECTION('ref_axis',(1.,0.,0.));
#12745=DIRECTION('center_axis',(0.,1.,0.));
#12746=DIRECTION('ref_axis',(1.,0.,0.));
#12747=DIRECTION('center_axis',(0.,1.,0.));
#12748=DIRECTION('ref_axis',(1.,0.,0.));
#12749=DIRECTION('center_axis',(0.,1.,0.));
#12750=DIRECTION('ref_axis',(1.,0.,0.));
#12751=DIRECTION('',(0.,-1.,0.));
#12752=DIRECTION('center_axis',(0.,1.,0.));
#12753=DIRECTION('ref_axis',(1.,0.,0.));
#12754=DIRECTION('center_axis',(0.,1.,0.));
#12755=DIRECTION('ref_axis',(1.,0.,0.));
#12756=DIRECTION('',(0.,-1.,0.));
#12757=DIRECTION('center_axis',(0.,1.,0.));
#12758=DIRECTION('ref_axis',(1.,0.,0.));
#12759=DIRECTION('center_axis',(0.,1.,0.));
#12760=DIRECTION('ref_axis',(1.,0.,0.));
#12761=DIRECTION('axis',(0.,0.,1.));
#12762=DIRECTION('refdir',(1.,0.,0.));
#12763=DIRECTION('center_axis',(-0.866025403784438,0.,0.5));
#12764=DIRECTION('ref_axis',(0.5,0.,0.866025403784438));
#12765=DIRECTION('',(-0.5,0.,-0.866025403784438));
#12766=DIRECTION('',(0.,1.,0.));
#12767=DIRECTION('',(-0.5,0.,-0.866025403784438));
#12768=DIRECTION('',(0.,1.,0.));
#12769=DIRECTION('center_axis',(-0.866025403784438,0.,-0.5));
#12770=DIRECTION('ref_axis',(-0.5,0.,0.866025403784438));
#12771=DIRECTION('',(0.5,0.,-0.866025403784438));
#12772=DIRECTION('',(0.5,0.,-0.866025403784438));
#12773=DIRECTION('',(0.,1.,0.));
#12774=DIRECTION('center_axis',(0.,0.,-1.));
#12775=DIRECTION('ref_axis',(-1.,0.,0.));
#12776=DIRECTION('',(1.,0.,0.));
#12777=DIRECTION('',(1.,0.,0.));
#12778=DIRECTION('',(0.,1.,0.));
#12779=DIRECTION('center_axis',(0.866025403784439,0.,-0.499999999999999));
#12780=DIRECTION('ref_axis',(-0.499999999999999,0.,-0.866025403784439));
#12781=DIRECTION('',(0.499999999999999,0.,0.866025403784439));
#12782=DIRECTION('',(0.499999999999999,0.,0.866025403784439));
#12783=DIRECTION('',(0.,1.,0.));
#12784=DIRECTION('center_axis',(0.866025403784439,0.,0.499999999999999));
#12785=DIRECTION('ref_axis',(0.499999999999999,0.,-0.866025403784439));
#12786=DIRECTION('',(-0.499999999999999,0.,0.866025403784439));
#12787=DIRECTION('',(-0.499999999999999,0.,0.866025403784439));
#12788=DIRECTION('',(0.,1.,0.));
#12789=DIRECTION('center_axis',(0.,0.,1.));
#12790=DIRECTION('ref_axis',(1.,0.,0.));
#12791=DIRECTION('',(-1.,0.,0.));
#12792=DIRECTION('',(-1.,0.,0.));
#12793=DIRECTION('center_axis',(0.,1.,0.));
#12794=DIRECTION('ref_axis',(1.,0.,0.));
#12795=DIRECTION('center_axis',(0.,1.,0.));
#12796=DIRECTION('ref_axis',(1.,0.,0.));
#12797=DIRECTION('center_axis',(0.,1.,0.));
#12798=DIRECTION('ref_axis',(1.,0.,0.));
#12799=DIRECTION('center_axis',(0.,1.,0.));
#12800=DIRECTION('ref_axis',(1.,0.,0.));
#12801=DIRECTION('center_axis',(0.,1.,0.));
#12802=DIRECTION('ref_axis',(1.,0.,0.));
#12803=DIRECTION('center_axis',(0.,1.,0.));
#12804=DIRECTION('ref_axis',(1.,0.,0.));
#12805=DIRECTION('',(0.,-1.,0.));
#12806=DIRECTION('center_axis',(0.,1.,0.));
#12807=DIRECTION('ref_axis',(1.,0.,0.));
#12808=DIRECTION('center_axis',(0.,1.,0.));
#12809=DIRECTION('ref_axis',(1.,0.,0.));
#12810=DIRECTION('',(0.,-1.,0.));
#12811=DIRECTION('center_axis',(0.,1.,0.));
#12812=DIRECTION('ref_axis',(1.,0.,0.));
#12813=DIRECTION('center_axis',(0.,1.,0.));
#12814=DIRECTION('ref_axis',(1.,0.,0.));
#12815=DIRECTION('axis',(0.,0.,1.));
#12816=DIRECTION('refdir',(1.,0.,0.));
#12817=DIRECTION('center_axis',(-0.866025403784439,0.,0.499999999999999));
#12818=DIRECTION('ref_axis',(0.499999999999999,0.,0.866025403784439));
#12819=DIRECTION('',(-0.499999999999999,0.,-0.866025403784439));
#12820=DIRECTION('',(0.,1.,0.));
#12821=DIRECTION('',(-0.499999999999999,0.,-0.866025403784439));
#12822=DIRECTION('',(0.,1.,0.));
#12823=DIRECTION('center_axis',(-0.86602540378444,0.,-0.499999999999998));
#12824=DIRECTION('ref_axis',(-0.499999999999998,0.,0.86602540378444));
#12825=DIRECTION('',(0.499999999999998,0.,-0.86602540378444));
#12826=DIRECTION('',(0.499999999999998,0.,-0.86602540378444));
#12827=DIRECTION('',(0.,1.,0.));
#12828=DIRECTION('center_axis',(0.,0.,-1.));
#12829=DIRECTION('ref_axis',(-1.,0.,0.));
#12830=DIRECTION('',(1.,0.,0.));
#12831=DIRECTION('',(1.,0.,0.));
#12832=DIRECTION('',(0.,1.,0.));
#12833=DIRECTION('center_axis',(0.866025403784438,0.,-0.5));
#12834=DIRECTION('ref_axis',(-0.5,0.,-0.866025403784438));
#12835=DIRECTION('',(0.5,0.,0.866025403784438));
#12836=DIRECTION('',(0.5,0.,0.866025403784438));
#12837=DIRECTION('',(0.,1.,0.));
#12838=DIRECTION('center_axis',(0.866025403784438,0.,0.5));
#12839=DIRECTION('ref_axis',(0.5,0.,-0.866025403784438));
#12840=DIRECTION('',(-0.5,0.,0.866025403784438));
#12841=DIRECTION('',(-0.5,0.,0.866025403784438));
#12842=DIRECTION('',(0.,1.,0.));
#12843=DIRECTION('center_axis',(0.,0.,1.));
#12844=DIRECTION('ref_axis',(1.,0.,0.));
#12845=DIRECTION('',(-1.,0.,0.));
#12846=DIRECTION('',(-1.,0.,0.));
#12847=DIRECTION('center_axis',(0.,1.,0.));
#12848=DIRECTION('ref_axis',(1.,0.,0.));
#12849=DIRECTION('center_axis',(0.,1.,0.));
#12850=DIRECTION('ref_axis',(1.,0.,0.));
#12851=DIRECTION('center_axis',(0.,1.,0.));
#12852=DIRECTION('ref_axis',(1.,0.,0.));
#12853=DIRECTION('center_axis',(0.,1.,0.));
#12854=DIRECTION('ref_axis',(1.,0.,0.));
#12855=DIRECTION('center_axis',(0.,1.,0.));
#12856=DIRECTION('ref_axis',(1.,0.,0.));
#12857=DIRECTION('center_axis',(0.,1.,0.));
#12858=DIRECTION('ref_axis',(1.,0.,0.));
#12859=DIRECTION('',(0.,-1.,0.));
#12860=DIRECTION('center_axis',(0.,1.,0.));
#12861=DIRECTION('ref_axis',(1.,0.,0.));
#12862=DIRECTION('center_axis',(0.,1.,0.));
#12863=DIRECTION('ref_axis',(1.,0.,0.));
#12864=DIRECTION('',(0.,-1.,0.));
#12865=DIRECTION('center_axis',(0.,1.,0.));
#12866=DIRECTION('ref_axis',(1.,0.,0.));
#12867=DIRECTION('center_axis',(0.,1.,0.));
#12868=DIRECTION('ref_axis',(1.,0.,0.));
#12869=DIRECTION('axis',(0.,0.,1.));
#12870=DIRECTION('refdir',(1.,0.,0.));
#12871=DIRECTION('center_axis',(-0.866025403784439,0.,0.499999999999999));
#12872=DIRECTION('ref_axis',(0.499999999999999,0.,0.866025403784439));
#12873=DIRECTION('',(-0.499999999999999,0.,-0.866025403784439));
#12874=DIRECTION('',(0.,1.,0.));
#12875=DIRECTION('',(-0.499999999999999,0.,-0.866025403784439));
#12876=DIRECTION('',(0.,1.,0.));
#12877=DIRECTION('center_axis',(-0.86602540378444,0.,-0.499999999999998));
#12878=DIRECTION('ref_axis',(-0.499999999999998,0.,0.86602540378444));
#12879=DIRECTION('',(0.499999999999998,0.,-0.86602540378444));
#12880=DIRECTION('',(0.499999999999998,0.,-0.86602540378444));
#12881=DIRECTION('',(0.,1.,0.));
#12882=DIRECTION('center_axis',(0.,0.,-1.));
#12883=DIRECTION('ref_axis',(-1.,0.,0.));
#12884=DIRECTION('',(1.,0.,0.));
#12885=DIRECTION('',(1.,0.,0.));
#12886=DIRECTION('',(0.,1.,0.));
#12887=DIRECTION('center_axis',(0.866025403784438,0.,-0.5));
#12888=DIRECTION('ref_axis',(-0.5,0.,-0.866025403784438));
#12889=DIRECTION('',(0.5,0.,0.866025403784438));
#12890=DIRECTION('',(0.5,0.,0.866025403784438));
#12891=DIRECTION('',(0.,1.,0.));
#12892=DIRECTION('center_axis',(0.866025403784438,0.,0.5));
#12893=DIRECTION('ref_axis',(0.5,0.,-0.866025403784438));
#12894=DIRECTION('',(-0.5,0.,0.866025403784438));
#12895=DIRECTION('',(-0.5,0.,0.866025403784438));
#12896=DIRECTION('',(0.,1.,0.));
#12897=DIRECTION('center_axis',(0.,0.,1.));
#12898=DIRECTION('ref_axis',(1.,0.,0.));
#12899=DIRECTION('',(-1.,0.,0.));
#12900=DIRECTION('',(-1.,0.,0.));
#12901=DIRECTION('center_axis',(0.,1.,0.));
#12902=DIRECTION('ref_axis',(1.,0.,0.));
#12903=DIRECTION('center_axis',(0.,1.,0.));
#12904=DIRECTION('ref_axis',(1.,0.,0.));
#12905=DIRECTION('center_axis',(0.,1.,0.));
#12906=DIRECTION('ref_axis',(1.,0.,0.));
#12907=DIRECTION('center_axis',(0.,1.,0.));
#12908=DIRECTION('ref_axis',(1.,0.,0.));
#12909=DIRECTION('center_axis',(0.,1.,0.));
#12910=DIRECTION('ref_axis',(1.,0.,0.));
#12911=DIRECTION('center_axis',(0.,1.,0.));
#12912=DIRECTION('ref_axis',(1.,0.,0.));
#12913=DIRECTION('',(0.,-1.,0.));
#12914=DIRECTION('center_axis',(0.,1.,0.));
#12915=DIRECTION('ref_axis',(1.,0.,0.));
#12916=DIRECTION('center_axis',(0.,1.,0.));
#12917=DIRECTION('ref_axis',(1.,0.,0.));
#12918=DIRECTION('',(0.,-1.,0.));
#12919=DIRECTION('center_axis',(0.,1.,0.));
#12920=DIRECTION('ref_axis',(1.,0.,0.));
#12921=DIRECTION('center_axis',(0.,1.,0.));
#12922=DIRECTION('ref_axis',(1.,0.,0.));
#12923=DIRECTION('axis',(0.,0.,1.));
#12924=DIRECTION('refdir',(1.,0.,0.));
#12925=DIRECTION('axis',(0.,0.,1.));
#12926=DIRECTION('refdir',(1.,0.,0.));
#12927=DIRECTION('center_axis',(0.,1.,0.));
#12928=DIRECTION('ref_axis',(1.,0.,0.));
#12929=DIRECTION('',(1.,0.,0.));
#12930=DIRECTION('center_axis',(0.,1.,0.));
#12931=DIRECTION('ref_axis',(1.,0.,0.));
#12932=DIRECTION('center_axis',(0.,1.,0.));
#12933=DIRECTION('ref_axis',(1.,0.,0.));
#12934=DIRECTION('',(0.,1.,0.));
#12935=DIRECTION('center_axis',(0.,-1.,0.));
#12936=DIRECTION('ref_axis',(1.,0.,0.));
#12937=DIRECTION('',(0.,-1.,0.));
#12938=DIRECTION('center_axis',(0.,1.,0.));
#12939=DIRECTION('ref_axis',(1.,0.,0.));
#12940=DIRECTION('',(0.,1.,0.));
#12941=DIRECTION('center_axis',(0.,-1.,0.));
#12942=DIRECTION('ref_axis',(1.,0.,0.));
#12943=DIRECTION('center_axis',(0.,1.,0.));
#12944=DIRECTION('ref_axis',(1.,0.,0.));
#12945=DIRECTION('center_axis',(0.,1.,0.));
#12946=DIRECTION('ref_axis',(1.,0.,0.));
#12947=DIRECTION('center_axis',(0.,1.,0.));
#12948=DIRECTION('ref_axis',(1.,0.,0.));
#12949=DIRECTION('',(0.,1.,0.));
#12950=DIRECTION('center_axis',(0.,-1.,0.));
#12951=DIRECTION('ref_axis',(1.,0.,0.));
#12952=DIRECTION('',(0.,-1.,0.));
#12953=DIRECTION('',(0.,1.,0.));
#12954=DIRECTION('center_axis',(0.,-1.,0.));
#12955=DIRECTION('ref_axis',(1.,0.,0.));
#12956=DIRECTION('center_axis',(0.,1.,0.));
#12957=DIRECTION('ref_axis',(1.,0.,0.));
#12958=DIRECTION('',(-1.,0.,0.));
#12959=DIRECTION('center_axis',(0.,1.,0.));
#12960=DIRECTION('ref_axis',(1.,0.,0.));
#12961=DIRECTION('',(-1.,0.,0.));
#12962=DIRECTION('center_axis',(0.,-1.,0.));
#12963=DIRECTION('ref_axis',(1.,0.,0.));
#12964=DIRECTION('',(-1.,0.,0.));
#12965=DIRECTION('center_axis',(6.12323399573677E-17,0.,1.));
#12966=DIRECTION('ref_axis',(1.,0.,0.));
#12967=DIRECTION('center_axis',(-1.22464679914735E-16,1.,0.));
#12968=DIRECTION('ref_axis',(-1.,-1.22464679914735E-16,0.));
#12969=DIRECTION('center_axis',(0.,1.,0.));
#12970=DIRECTION('ref_axis',(0.,0.,1.));
#12971=DIRECTION('',(1.,0.,0.));
#12972=DIRECTION('',(0.9045256429963,0.,0.426419231698256));
#12973=DIRECTION('center_axis',(0.,1.,0.));
#12974=DIRECTION('ref_axis',(1.,0.,0.));
#12975=DIRECTION('center_axis',(0.,1.,0.));
#12976=DIRECTION('ref_axis',(0.,0.,1.));
#12977=DIRECTION('',(1.,0.,0.));
#12978=DIRECTION('center_axis',(0.,1.,0.));
#12979=DIRECTION('ref_axis',(1.,0.,0.));
#12980=DIRECTION('',(0.9045256429963,0.,-0.426419231698256));
#12981=DIRECTION('center_axis',(0.,-1.,0.));
#12982=DIRECTION('ref_axis',(0.,0.,-1.));
#12983=DIRECTION('',(-1.,0.,0.));
#12984=DIRECTION('center_axis',(0.,-1.,0.));
#12985=DIRECTION('ref_axis',(1.,0.,0.));
#12986=DIRECTION('',(-0.9045256429963,0.,-0.426419231698256));
#12987=DIRECTION('center_axis',(-0.426419231698256,0.,0.9045256429963));
#12988=DIRECTION('ref_axis',(0.9045256429963,0.,0.426419231698256));
#12989=DIRECTION('',(0.,1.,0.));
#12990=DIRECTION('',(0.,-1.,0.));
#12991=DIRECTION('center_axis',(0.,-1.,0.));
#12992=DIRECTION('ref_axis',(0.,0.,-1.));
#12993=DIRECTION('',(-1.,0.,0.));
#12994=DIRECTION('',(-0.9045256429963,0.,0.426419231698256));
#12995=DIRECTION('center_axis',(0.,-1.,0.));
#12996=DIRECTION('ref_axis',(1.,0.,0.));
#12997=DIRECTION('center_axis',(0.426419231698256,0.,0.9045256429963));
#12998=DIRECTION('ref_axis',(0.9045256429963,0.,-0.426419231698256));
#12999=DIRECTION('',(0.,-1.,0.));
#13000=DIRECTION('',(0.,1.,0.));
#13001=DIRECTION('center_axis',(0.,0.,1.));
#13002=DIRECTION('ref_axis',(1.,0.,0.));
#13003=DIRECTION('',(0.,-1.,0.));
#13004=DIRECTION('',(1.,0.,0.));
#13005=DIRECTION('',(0.,1.,0.));
#13006=DIRECTION('',(-1.,0.,0.));
#13007=DIRECTION('',(0.,1.,0.));
#13008=DIRECTION('',(0.,1.,0.));
#13009=DIRECTION('',(1.,0.,0.));
#13010=DIRECTION('',(1.,0.,0.));
#13011=DIRECTION('',(0.,-1.,0.));
#13012=DIRECTION('',(0.,-1.,0.));
#13013=DIRECTION('center_axis',(0.,0.,-1.));
#13014=DIRECTION('ref_axis',(1.,0.,0.));
#13015=DIRECTION('center_axis',(0.,0.,-1.));
#13016=DIRECTION('ref_axis',(1.,0.,0.));
#13017=DIRECTION('center_axis',(0.,1.,0.));
#13018=DIRECTION('ref_axis',(1.,0.,0.));
#13019=DIRECTION('center_axis',(0.,-1.,0.));
#13020=DIRECTION('ref_axis',(1.,0.,0.));
#13021=DIRECTION('',(0.,-1.,0.));
#13022=DIRECTION('center_axis',(0.,1.,0.));
#13023=DIRECTION('ref_axis',(1.,0.,0.));
#13024=DIRECTION('',(0.,1.,0.));
#13025=DIRECTION('center_axis',(0.,1.,0.));
#13026=DIRECTION('ref_axis',(6.12323399573677E-17,0.,1.));
#13027=DIRECTION('center_axis',(0.,1.,0.));
#13028=DIRECTION('ref_axis',(1.,0.,0.));
#13029=DIRECTION('center_axis',(0.,1.,0.));
#13030=DIRECTION('ref_axis',(1.,0.,0.));
#13031=DIRECTION('center_axis',(0.,1.,0.));
#13032=DIRECTION('ref_axis',(-1.,0.,0.));
#13033=DIRECTION('',(-1.,0.,0.));
#13034=DIRECTION('',(0.,0.,1.));
#13035=DIRECTION('',(-1.,0.,0.));
#13036=DIRECTION('',(0.,0.,1.));
#13037=DIRECTION('',(-1.,0.,0.));
#13038=DIRECTION('center_axis',(0.,0.,1.));
#13039=DIRECTION('ref_axis',(1.,0.,0.));
#13040=DIRECTION('',(1.,0.,0.));
#13041=DIRECTION('',(0.,-1.,0.));
#13042=DIRECTION('center_axis',(1.,0.,0.));
#13043=DIRECTION('ref_axis',(0.,1.,0.));
#13044=DIRECTION('',(0.,1.,0.));
#13045=DIRECTION('',(0.,0.,1.));
#13046=DIRECTION('',(0.,1.,0.));
#13047=DIRECTION('center_axis',(0.,-1.,0.));
#13048=DIRECTION('ref_axis',(1.,0.,0.));
#13049=DIRECTION('',(1.,0.,0.));
#13050=DIRECTION('',(1.,0.,0.));
#13051=DIRECTION('',(0.,0.,1.));
#13052=DIRECTION('center_axis',(-1.,0.,0.));
#13053=DIRECTION('ref_axis',(0.,-1.,0.));
#13054=DIRECTION('',(0.,-1.,0.));
#13055=DIRECTION('center_axis',(0.,0.,1.));
#13056=DIRECTION('ref_axis',(1.,0.,0.));
#13057=DIRECTION('center_axis',(0.,0.,1.));
#13058=DIRECTION('ref_axis',(1.,0.,0.));
#13059=DIRECTION('center_axis',(0.,0.,1.));
#13060=DIRECTION('ref_axis',(1.,0.,0.));
#13061=DIRECTION('',(0.,0.,1.));
#13062=DIRECTION('center_axis',(0.,0.,1.));
#13063=DIRECTION('ref_axis',(1.,0.,0.));
#13064=DIRECTION('center_axis',(0.,0.,1.));
#13065=DIRECTION('ref_axis',(1.,0.,0.));
#13066=DIRECTION('',(0.,0.,1.));
#13067=DIRECTION('center_axis',(0.,1.,0.));
#13068=DIRECTION('ref_axis',(-1.,0.,0.));
#13069=DIRECTION('',(-1.,0.,0.));
#13070=DIRECTION('',(0.,0.,1.));
#13071=DIRECTION('',(0.,0.,1.));
#13072=DIRECTION('center_axis',(1.,0.,0.));
#13073=DIRECTION('ref_axis',(0.,1.,0.));
#13074=DIRECTION('',(0.,1.,0.));
#13075=DIRECTION('',(0.,0.,1.));
#13076=DIRECTION('center_axis',(0.,-1.,0.));
#13077=DIRECTION('ref_axis',(1.,0.,0.));
#13078=DIRECTION('',(1.,0.,0.));
#13079=DIRECTION('',(0.,0.,1.));
#13080=DIRECTION('center_axis',(-1.,0.,0.));
#13081=DIRECTION('ref_axis',(0.,-1.,0.));
#13082=DIRECTION('',(0.,-1.,0.));
#13083=DIRECTION('center_axis',(0.,0.,1.));
#13084=DIRECTION('ref_axis',(1.,0.,0.));
#13085=DIRECTION('axis',(0.,0.,1.));
#13086=DIRECTION('refdir',(1.,0.,0.));
#13087=DIRECTION('center_axis',(0.,-1.,0.));
#13088=DIRECTION('ref_axis',(1.,0.,0.));
#13089=DIRECTION('center_axis',(0.,-1.,0.));
#13090=DIRECTION('ref_axis',(1.,0.,0.));
#13091=DIRECTION('',(0.,1.,0.));
#13092=DIRECTION('center_axis',(0.,-1.,0.));
#13093=DIRECTION('ref_axis',(1.,0.,0.));
#13094=DIRECTION('center_axis',(0.,1.,0.));
#13095=DIRECTION('ref_axis',(0.,0.,1.));
#13096=DIRECTION('center_axis',(0.,-1.,0.));
#13097=DIRECTION('ref_axis',(1.,0.,0.));
#13098=DIRECTION('center_axis',(6.12323399573677E-17,0.,1.));
#13099=DIRECTION('ref_axis',(1.,0.,0.));
#13100=DIRECTION('center_axis',(1.22464679914735E-16,-1.,0.));
#13101=DIRECTION('ref_axis',(-1.,-1.22464679914735E-16,0.));
#13102=DIRECTION('center_axis',(0.,-1.,0.));
#13103=DIRECTION('ref_axis',(1.,0.,0.));
#13104=DIRECTION('center_axis',(0.,-1.,0.));
#13105=DIRECTION('ref_axis',(0.,0.,-1.));
#13106=DIRECTION('center_axis',(-0.866025403784438,0.,-0.5));
#13107=DIRECTION('ref_axis',(-0.5,0.,0.866025403784438));
#13108=DIRECTION('',(-0.866025403784438,0.,-0.5));
#13109=DIRECTION('center_axis',(-0.866025403784438,0.,-0.5));
#13110=DIRECTION('ref_axis',(-0.5,0.,0.866025403784438));
#13111=DIRECTION('',(-0.866025403784438,0.,-0.5));
#13112=DIRECTION('center_axis',(0.,-1.,0.));
#13113=DIRECTION('ref_axis',(1.,0.,0.));
#13114=DIRECTION('center_axis',(0.,-1.,0.));
#13115=DIRECTION('ref_axis',(1.,0.,0.));
#13116=DIRECTION('',(0.,1.,0.));
#13117=DIRECTION('center_axis',(0.,-1.,0.));
#13118=DIRECTION('ref_axis',(1.,0.,0.));
#13119=DIRECTION('center_axis',(0.866025403784439,0.,-0.5));
#13120=DIRECTION('ref_axis',(-0.5,0.,-0.866025403784439));
#13121=DIRECTION('',(0.866025403784439,0.,-0.5));
#13122=DIRECTION('center_axis',(0.866025403784439,0.,-0.5));
#13123=DIRECTION('ref_axis',(-0.5,0.,-0.866025403784439));
#13124=DIRECTION('',(0.866025403784439,0.,-0.5));
#13125=DIRECTION('center_axis',(0.,0.,1.));
#13126=DIRECTION('ref_axis',(1.,0.,0.));
#13127=DIRECTION('',(0.,0.,1.));
#13128=DIRECTION('center_axis',(0.,0.,1.));
#13129=DIRECTION('ref_axis',(1.,0.,0.));
#13130=DIRECTION('',(0.,0.,1.));
#13131=DIRECTION('center_axis',(0.,1.,0.));
#13132=DIRECTION('ref_axis',(0.,0.,1.));
#13133=DIRECTION('center_axis',(0.,-1.,0.));
#13134=DIRECTION('ref_axis',(1.,0.,0.));
#13135=DIRECTION('center_axis',(0.,1.,0.));
#13136=DIRECTION('ref_axis',(0.,0.,1.));
#13137=DIRECTION('center_axis',(0.,-1.,0.));
#13138=DIRECTION('ref_axis',(1.,0.,0.));
#13139=DIRECTION('center_axis',(0.,-1.,0.));
#13140=DIRECTION('ref_axis',(1.,0.,0.));
#13141=DIRECTION('center_axis',(0.,-1.,0.));
#13142=DIRECTION('ref_axis',(1.,0.,0.));
#13143=DIRECTION('',(0.,1.,0.));
#13144=DIRECTION('center_axis',(0.,-1.,0.));
#13145=DIRECTION('ref_axis',(0.,0.,-1.));
#13146=DIRECTION('center_axis',(0.,-1.,0.));
#13147=DIRECTION('ref_axis',(1.,0.,0.));
#13148=DIRECTION('center_axis',(0.,-1.,0.));
#13149=DIRECTION('ref_axis',(1.,0.,0.));
#13150=DIRECTION('',(0.,1.,0.));
#13151=DIRECTION('',(0.,0.,1.));
#13152=DIRECTION('',(1.,0.,0.));
#13153=DIRECTION('',(0.,0.,1.));
#13154=DIRECTION('',(1.,0.,0.));
#13155=DIRECTION('axis',(0.,0.,1.));
#13156=DIRECTION('refdir',(1.,0.,0.));
#13157=DIRECTION('center_axis',(0.,1.,0.));
#13158=DIRECTION('ref_axis',(1.,0.,0.));
#13159=DIRECTION('center_axis',(0.,-1.,0.));
#13160=DIRECTION('ref_axis',(1.,0.,0.));
#13161=DIRECTION('',(0.,-1.,0.));
#13162=DIRECTION('center_axis',(0.,-1.,0.));
#13163=DIRECTION('ref_axis',(1.,0.,0.));
#13164=DIRECTION('center_axis',(0.,1.,0.));
#13165=DIRECTION('ref_axis',(1.,0.,0.));
#13166=DIRECTION('center_axis',(0.,1.,0.));
#13167=DIRECTION('ref_axis',(1.,0.,0.));
#13168=DIRECTION('',(0.,-1.,0.));
#13169=DIRECTION('center_axis',(0.,1.,0.));
#13170=DIRECTION('ref_axis',(1.,0.,0.));
#13171=DIRECTION('center_axis',(0.,1.,0.));
#13172=DIRECTION('ref_axis',(1.,0.,0.));
#13173=DIRECTION('center_axis',(0.,1.,0.));
#13174=DIRECTION('ref_axis',(1.,0.,0.));
#13175=DIRECTION('axis',(0.,0.,1.));
#13176=DIRECTION('refdir',(1.,0.,0.));
#13177=DIRECTION('center_axis',(0.866025403784439,0.,-0.5));
#13178=DIRECTION('ref_axis',(0.5,0.,0.866025403784439));
#13179=DIRECTION('',(-0.5,0.,-0.866025403784439));
#13180=DIRECTION('',(0.,-1.,0.));
#13181=DIRECTION('',(0.5,0.,0.866025403784439));
#13182=DIRECTION('',(0.,-1.,0.));
#13183=DIRECTION('center_axis',(1.60246890531964E-16,0.,-1.));
#13184=DIRECTION('ref_axis',(1.,0.,1.60246890531964E-16));
#13185=DIRECTION('',(-1.,0.,-1.60246890531964E-16));
#13186=DIRECTION('',(0.,-1.,0.));
#13187=DIRECTION('',(1.,0.,1.60246890531964E-16));
#13188=DIRECTION('center_axis',(-0.866025403784439,0.,-0.5));
#13189=DIRECTION('ref_axis',(0.5,0.,-0.866025403784439));
#13190=DIRECTION('',(-0.5,0.,0.866025403784439));
#13191=DIRECTION('',(0.,-1.,0.));
#13192=DIRECTION('',(0.5,0.,-0.866025403784439));
#13193=DIRECTION('center_axis',(-0.866025403784439,0.,0.5));
#13194=DIRECTION('ref_axis',(-0.5,0.,-0.866025403784439));
#13195=DIRECTION('',(0.5,0.,0.866025403784439));
#13196=DIRECTION('',(0.,-1.,0.));
#13197=DIRECTION('',(-0.5,0.,-0.866025403784439));
#13198=DIRECTION('center_axis',(-1.60246890531964E-16,0.,1.));
#13199=DIRECTION('ref_axis',(-1.,0.,-1.60246890531964E-16));
#13200=DIRECTION('',(1.,0.,1.60246890531964E-16));
#13201=DIRECTION('',(0.,-1.,0.));
#13202=DIRECTION('',(-1.,0.,-1.60246890531964E-16));
#13203=DIRECTION('center_axis',(0.866025403784439,0.,0.5));
#13204=DIRECTION('ref_axis',(-0.5,0.,0.866025403784439));
#13205=DIRECTION('',(0.5,0.,-0.866025403784439));
#13206=DIRECTION('',(-0.5,0.,0.866025403784439));
#13207=DIRECTION('center_axis',(0.,1.,0.));
#13208=DIRECTION('ref_axis',(1.,0.,0.));
#13209=DIRECTION('center_axis',(0.,-1.,0.));
#13210=DIRECTION('ref_axis',(0.,0.,-1.));
#13211=DIRECTION('center_axis',(0.,1.,0.));
#13212=DIRECTION('ref_axis',(1.,0.,0.));
#13213=DIRECTION('center_axis',(0.,1.,0.));
#13214=DIRECTION('ref_axis',(1.,0.,0.));
#13215=DIRECTION('center_axis',(0.,1.,0.));
#13216=DIRECTION('ref_axis',(0.,0.,1.));
#13217=DIRECTION('center_axis',(0.,-1.,0.));
#13218=DIRECTION('ref_axis',(1.,0.,0.));
#13219=DIRECTION('center_axis',(0.,-1.,0.));
#13220=DIRECTION('ref_axis',(1.,0.,0.));
#13221=DIRECTION('center_axis',(0.,-1.,0.));
#13222=DIRECTION('ref_axis',(1.,0.,0.));
#13223=DIRECTION('',(0.707106781186548,0.707106781186547,8.65956056235493E-17));
#13224=DIRECTION('center_axis',(0.,-1.,0.));
#13225=DIRECTION('ref_axis',(1.,0.,0.));
#13226=DIRECTION('center_axis',(0.,-1.,0.));
#13227=DIRECTION('ref_axis',(1.,0.,0.));
#13228=DIRECTION('',(0.,1.,0.));
#13229=DIRECTION('center_axis',(0.,1.,0.));
#13230=DIRECTION('ref_axis',(1.,0.,0.));
#13231=DIRECTION('center_axis',(0.,-1.,0.));
#13232=DIRECTION('ref_axis',(1.,0.,0.));
#13233=DIRECTION('',(-0.707106781186548,0.707106781186547,-8.65956056235494E-17));
#13234=DIRECTION('center_axis',(0.,-1.,0.));
#13235=DIRECTION('ref_axis',(0.,0.,-1.));
#13236=DIRECTION('center_axis',(0.,-1.,0.));
#13237=DIRECTION('ref_axis',(1.,0.,0.));
#13238=DIRECTION('center_axis',(0.,1.,0.));
#13239=DIRECTION('ref_axis',(1.,0.,0.));
#13240=DIRECTION('center_axis',(0.,1.,0.));
#13241=DIRECTION('ref_axis',(1.,0.,0.));
#13242=DIRECTION('',(-0.447213595499958,0.894427190999916,-5.47678698264203E-17));
#13243=DIRECTION('center_axis',(0.,-1.,0.));
#13244=DIRECTION('ref_axis',(1.,0.,0.));
#13245=DIRECTION('',(0.,1.,0.));
#13246=DIRECTION('axis',(0.,0.,1.));
#13247=DIRECTION('refdir',(1.,0.,0.));
#13248=DIRECTION('center_axis',(0.866025403784439,0.,-0.5));
#13249=DIRECTION('ref_axis',(0.5,0.,0.866025403784439));
#13250=DIRECTION('',(-0.5,0.,-0.866025403784439));
#13251=DIRECTION('',(0.,-1.,0.));
#13252=DIRECTION('',(0.5,0.,0.866025403784439));
#13253=DIRECTION('',(0.,-1.,0.));
#13254=DIRECTION('center_axis',(1.20185167898973E-16,0.,-1.));
#13255=DIRECTION('ref_axis',(1.,0.,1.20185167898973E-16));
#13256=DIRECTION('',(-1.,0.,-1.20185167898973E-16));
#13257=DIRECTION('',(0.,-1.,0.));
#13258=DIRECTION('',(1.,0.,1.20185167898973E-16));
#13259=DIRECTION('center_axis',(-0.866025403784439,0.,-0.5));
#13260=DIRECTION('ref_axis',(0.5,0.,-0.866025403784439));
#13261=DIRECTION('',(-0.5,0.,0.866025403784439));
#13262=DIRECTION('',(0.,-1.,0.));
#13263=DIRECTION('',(0.5,0.,-0.866025403784439));
#13264=DIRECTION('center_axis',(-0.866025403784439,0.,0.5));
#13265=DIRECTION('ref_axis',(-0.5,0.,-0.866025403784439));
#13266=DIRECTION('',(0.5,0.,0.866025403784439));
#13267=DIRECTION('',(0.,-1.,0.));
#13268=DIRECTION('',(-0.5,0.,-0.866025403784439));
#13269=DIRECTION('center_axis',(-2.40370335797945E-16,0.,1.));
#13270=DIRECTION('ref_axis',(-1.,0.,-2.40370335797945E-16));
#13271=DIRECTION('',(1.,0.,2.40370335797945E-16));
#13272=DIRECTION('',(0.,-1.,0.));
#13273=DIRECTION('',(-1.,0.,-2.40370335797945E-16));
#13274=DIRECTION('center_axis',(0.866025403784439,0.,0.5));
#13275=DIRECTION('ref_axis',(-0.5,0.,0.866025403784439));
#13276=DIRECTION('',(0.5,0.,-0.866025403784439));
#13277=DIRECTION('',(-0.5,0.,0.866025403784439));
#13278=DIRECTION('center_axis',(0.,1.,0.));
#13279=DIRECTION('ref_axis',(1.,0.,0.));
#13280=DIRECTION('center_axis',(0.,-1.,0.));
#13281=DIRECTION('ref_axis',(0.,0.,-1.));
#13282=DIRECTION('center_axis',(0.,1.,0.));
#13283=DIRECTION('ref_axis',(1.,0.,0.));
#13284=DIRECTION('center_axis',(0.,1.,0.));
#13285=DIRECTION('ref_axis',(1.,0.,0.));
#13286=DIRECTION('center_axis',(0.,1.,0.));
#13287=DIRECTION('ref_axis',(0.,0.,1.));
#13288=DIRECTION('center_axis',(0.,-1.,0.));
#13289=DIRECTION('ref_axis',(1.,0.,0.));
#13290=DIRECTION('center_axis',(0.,-1.,0.));
#13291=DIRECTION('ref_axis',(1.,0.,0.));
#13292=DIRECTION('center_axis',(0.,-1.,0.));
#13293=DIRECTION('ref_axis',(1.,0.,0.));
#13294=DIRECTION('',(0.707106781186548,0.707106781186547,8.65956056235493E-17));
#13295=DIRECTION('center_axis',(0.,-1.,0.));
#13296=DIRECTION('ref_axis',(1.,0.,0.));
#13297=DIRECTION('center_axis',(0.,-1.,0.));
#13298=DIRECTION('ref_axis',(1.,0.,0.));
#13299=DIRECTION('',(0.,1.,0.));
#13300=DIRECTION('center_axis',(0.,1.,0.));
#13301=DIRECTION('ref_axis',(1.,0.,0.));
#13302=DIRECTION('center_axis',(0.,-1.,0.));
#13303=DIRECTION('ref_axis',(1.,0.,0.));
#13304=DIRECTION('',(-0.707106781186547,0.707106781186548,-8.65956056235493E-17));
#13305=DIRECTION('center_axis',(0.,-1.,0.));
#13306=DIRECTION('ref_axis',(0.,0.,-1.));
#13307=DIRECTION('center_axis',(0.,-1.,0.));
#13308=DIRECTION('ref_axis',(1.,0.,0.));
#13309=DIRECTION('center_axis',(0.,1.,0.));
#13310=DIRECTION('ref_axis',(1.,0.,0.));
#13311=DIRECTION('center_axis',(0.,1.,0.));
#13312=DIRECTION('ref_axis',(1.,0.,0.));
#13313=DIRECTION('',(-0.447213595499958,0.894427190999916,-5.47678698264203E-17));
#13314=DIRECTION('center_axis',(0.,-1.,0.));
#13315=DIRECTION('ref_axis',(1.,0.,0.));
#13316=DIRECTION('',(0.,1.,0.));
#13317=DIRECTION('',(0.,0.,1.));
#13318=DIRECTION('',(1.,0.,0.));
#13319=DIRECTION('',(0.,0.,1.));
#13320=DIRECTION('',(1.,0.,0.));
#13321=DIRECTION('',(0.,0.,1.));
#13322=DIRECTION('',(1.,0.,0.));
#13323=DIRECTION('',(0.,0.,1.));
#13324=DIRECTION('',(1.,0.,0.));
#13325=DIRECTION('',(0.,0.,1.));
#13326=DIRECTION('',(1.,0.,0.));
#13327=DIRECTION('',(0.,0.,1.));
#13328=DIRECTION('',(1.,0.,0.));
#13329=DIRECTION('',(0.,0.,1.));
#13330=DIRECTION('',(1.,0.,0.));
#13331=DIRECTION('',(0.,0.,1.));
#13332=DIRECTION('',(1.,0.,0.));
#13333=DIRECTION('',(0.,0.,1.));
#13334=DIRECTION('',(1.,0.,0.));
#13335=DIRECTION('',(0.,0.,1.));
#13336=DIRECTION('',(1.,0.,0.));
#13337=DIRECTION('',(0.,0.,1.));
#13338=DIRECTION('',(1.,0.,0.));
#13339=DIRECTION('',(0.,0.,1.));
#13340=DIRECTION('',(1.,0.,0.));
#13341=DIRECTION('',(0.,0.,1.));
#13342=DIRECTION('',(1.,0.,0.));
#13343=DIRECTION('',(0.,0.,1.));
#13344=DIRECTION('',(1.,0.,0.));
#13345=DIRECTION('',(0.,-1.,2.22044604925031E-16));
#13346=DIRECTION('',(1.,0.,0.));
#13347=DIRECTION('',(0.,-1.,2.22044604925031E-16));
#13348=DIRECTION('',(1.,0.,0.));
#13349=DIRECTION('',(0.,-1.,2.22044604925031E-16));
#13350=DIRECTION('',(1.,0.,0.));
#13351=DIRECTION('',(0.,-1.,2.22044604925031E-16));
#13352=DIRECTION('',(1.,0.,0.));
#13353=DIRECTION('',(0.,0.,1.));
#13354=DIRECTION('',(1.,0.,0.));
#13355=DIRECTION('',(0.,-1.,2.22044604925031E-16));
#13356=DIRECTION('',(1.,0.,0.));
#13357=DIRECTION('',(0.,-1.,2.22044604925031E-16));
#13358=DIRECTION('',(1.,0.,0.));
#13359=DIRECTION('',(0.,-1.,2.22044604925031E-16));
#13360=DIRECTION('',(1.,0.,0.));
#13361=DIRECTION('',(0.,-1.,2.22044604925031E-16));
#13362=DIRECTION('',(1.,0.,0.));
#13363=DIRECTION('',(0.,-1.,2.22044604925031E-16));
#13364=DIRECTION('',(1.,0.,0.));
#13365=DIRECTION('',(0.,-1.,2.22044604925031E-16));
#13366=DIRECTION('',(1.,0.,0.));
#13367=DIRECTION('axis',(0.,0.,1.));
#13368=DIRECTION('refdir',(1.,0.,0.));
#13369=DIRECTION('axis',(0.,0.,1.));
#13370=DIRECTION('refdir',(1.,0.,0.));
#13371=DIRECTION('center_axis',(-1.,0.,0.));
#13372=DIRECTION('ref_axis',(0.,0.,1.));
#13373=DIRECTION('',(0.,-1.,0.));
#13374=DIRECTION('',(0.,0.,1.));
#13375=DIRECTION('',(0.,1.,0.));
#13376=DIRECTION('',(0.,0.,-1.));
#13377=DIRECTION('center_axis',(0.,1.,0.));
#13378=DIRECTION('ref_axis',(1.,0.,0.));
#13379=DIRECTION('center_axis',(0.,-1.,0.));
#13380=DIRECTION('ref_axis',(1.,0.,0.));
#13381=DIRECTION('',(-1.,0.,0.));
#13382=DIRECTION('',(0.,0.,1.));
#13383=DIRECTION('center_axis',(1.,0.,0.));
#13384=DIRECTION('ref_axis',(0.,0.,-1.));
#13385=DIRECTION('',(0.,1.,0.));
#13386=DIRECTION('',(0.,1.,0.));
#13387=DIRECTION('',(0.,0.,-1.));
#13388=DIRECTION('center_axis',(0.,0.,1.));
#13389=DIRECTION('ref_axis',(1.,0.,0.));
#13390=DIRECTION('',(1.,0.,0.));
#13391=DIRECTION('center_axis',(0.,1.,0.));
#13392=DIRECTION('ref_axis',(0.,0.,1.));
#13393=DIRECTION('center_axis',(0.,1.,0.));
#13394=DIRECTION('ref_axis',(1.,0.,0.));
#13395=DIRECTION('center_axis',(0.,1.,0.));
#13396=DIRECTION('ref_axis',(1.,0.,0.));
#13397=DIRECTION('center_axis',(0.,1.,0.));
#13398=DIRECTION('ref_axis',(1.,0.,0.));
#13399=DIRECTION('',(0.,1.,0.));
#13400=DIRECTION('center_axis',(0.,-1.,0.));
#13401=DIRECTION('ref_axis',(1.,0.,0.));
#13402=DIRECTION('center_axis',(0.,1.,0.));
#13403=DIRECTION('ref_axis',(1.,0.,0.));
#13404=DIRECTION('center_axis',(0.,1.,0.));
#13405=DIRECTION('ref_axis',(1.,0.,0.));
#13406=DIRECTION('center_axis',(0.,1.,0.));
#13407=DIRECTION('ref_axis',(1.,0.,0.));
#13408=DIRECTION('',(0.,-1.,0.));
#13409=DIRECTION('center_axis',(0.,1.,0.));
#13410=DIRECTION('ref_axis',(1.,0.,0.));
#13411=DIRECTION('center_axis',(0.,1.,0.));
#13412=DIRECTION('ref_axis',(1.,0.,0.));
#13413=DIRECTION('center_axis',(0.,1.,0.));
#13414=DIRECTION('ref_axis',(1.,0.,0.));
#13415=DIRECTION('axis',(0.,0.,1.));
#13416=DIRECTION('refdir',(1.,0.,0.));
#13417=DIRECTION('center_axis',(0.,1.,0.));
#13418=DIRECTION('ref_axis',(1.,0.,0.));
#13419=DIRECTION('center_axis',(0.,1.,0.));
#13420=DIRECTION('ref_axis',(1.,0.,0.));
#13421=DIRECTION('',(0.,-1.,0.));
#13422=DIRECTION('center_axis',(0.,1.,0.));
#13423=DIRECTION('ref_axis',(1.,0.,0.));
#13424=DIRECTION('center_axis',(0.,1.,0.));
#13425=DIRECTION('ref_axis',(1.,0.,0.));
#13426=DIRECTION('center_axis',(0.,1.,0.));
#13427=DIRECTION('ref_axis',(1.,0.,0.));
#13428=DIRECTION('axis',(0.,0.,1.));
#13429=DIRECTION('refdir',(1.,0.,0.));
#13430=DIRECTION('center_axis',(0.,0.,1.));
#13431=DIRECTION('ref_axis',(1.,0.,0.));
#13432=DIRECTION('',(0.,1.,0.));
#13433=DIRECTION('center_axis',(0.,0.,1.));
#13434=DIRECTION('ref_axis',(1.,0.,0.));
#13435=DIRECTION('center_axis',(0.,0.,1.));
#13436=DIRECTION('ref_axis',(1.,0.,0.));
#13437=DIRECTION('center_axis',(0.,0.,1.));
#13438=DIRECTION('ref_axis',(1.,0.,0.));
#13439=DIRECTION('',(0.,0.,1.));
#13440=DIRECTION('center_axis',(0.,0.,1.));
#13441=DIRECTION('ref_axis',(1.,0.,0.));
#13442=DIRECTION('center_axis',(0.,0.,1.));
#13443=DIRECTION('ref_axis',(1.,0.,0.));
#13444=DIRECTION('',(0.,-1.,0.));
#13445=DIRECTION('center_axis',(0.,1.,0.));
#13446=DIRECTION('ref_axis',(1.,0.,0.));
#13447=DIRECTION('center_axis',(0.,-1.,0.));
#13448=DIRECTION('ref_axis',(1.,0.,0.));
#13449=DIRECTION('',(0.,-1.,0.));
#13450=DIRECTION('center_axis',(0.,-1.,0.));
#13451=DIRECTION('ref_axis',(1.,0.,0.));
#13452=DIRECTION('center_axis',(0.,1.,0.));
#13453=DIRECTION('ref_axis',(1.,0.,0.));
#13454=DIRECTION('center_axis',(0.,1.,0.));
#13455=DIRECTION('ref_axis',(1.,0.,0.));
#13456=DIRECTION('',(0.,-1.,0.));
#13457=DIRECTION('center_axis',(0.,1.,0.));
#13458=DIRECTION('ref_axis',(1.,0.,0.));
#13459=DIRECTION('center_axis',(0.,1.,0.));
#13460=DIRECTION('ref_axis',(1.,0.,0.));
#13461=DIRECTION('center_axis',(0.,1.,0.));
#13462=DIRECTION('ref_axis',(1.,0.,0.));
#13463=DIRECTION('axis',(0.,0.,1.));
#13464=DIRECTION('refdir',(1.,0.,0.));
#13465=DIRECTION('center_axis',(0.,0.,1.));
#13466=DIRECTION('ref_axis',(1.,0.,0.));
#13467=DIRECTION('',(0.,1.,0.));
#13468=DIRECTION('center_axis',(0.,0.,1.));
#13469=DIRECTION('ref_axis',(1.,0.,0.));
#13470=DIRECTION('center_axis',(0.,0.,1.));
#13471=DIRECTION('ref_axis',(1.,0.,0.));
#13472=DIRECTION('center_axis',(0.,0.,1.));
#13473=DIRECTION('ref_axis',(1.,0.,0.));
#13474=DIRECTION('',(0.,0.,1.));
#13475=DIRECTION('center_axis',(0.,0.,1.));
#13476=DIRECTION('ref_axis',(1.,0.,0.));
#13477=DIRECTION('center_axis',(0.,0.,1.));
#13478=DIRECTION('ref_axis',(1.,0.,0.));
#13479=DIRECTION('',(0.,-1.,0.));
#13480=DIRECTION('center_axis',(-1.,0.,0.));
#13481=DIRECTION('ref_axis',(0.,0.,1.));
#13482=DIRECTION('',(0.,0.,1.));
#13483=DIRECTION('',(0.,1.,0.));
#13484=DIRECTION('',(0.,0.,-1.));
#13485=DIRECTION('',(0.,1.,0.));
#13486=DIRECTION('center_axis',(0.,0.,-1.));
#13487=DIRECTION('ref_axis',(-1.,0.,0.));
#13488=DIRECTION('',(-1.,0.,0.));
#13489=DIRECTION('',(0.,1.,0.));
#13490=DIRECTION('',(1.,0.,0.));
#13491=DIRECTION('center_axis',(1.,0.,0.));
#13492=DIRECTION('ref_axis',(0.,0.,-1.));
#13493=DIRECTION('',(0.,0.,-1.));
#13494=DIRECTION('',(0.,-1.,0.));
#13495=DIRECTION('',(0.,0.,1.));
#13496=DIRECTION('center_axis',(0.,1.,0.));
#13497=DIRECTION('ref_axis',(1.,0.,0.));
#13498=DIRECTION('center_axis',(0.,1.,0.));
#13499=DIRECTION('ref_axis',(1.,0.,0.));
#13500=DIRECTION('center_axis',(0.,-1.,0.));
#13501=DIRECTION('ref_axis',(1.,0.,0.));
#13502=DIRECTION('center_axis',(0.,1.,0.));
#13503=DIRECTION('ref_axis',(-1.83697019872103E-16,0.,1.));
#13504=DIRECTION('center_axis',(0.,-1.,0.));
#13505=DIRECTION('ref_axis',(1.,0.,0.));
#13506=DIRECTION('center_axis',(0.,1.,0.));
#13507=DIRECTION('ref_axis',(1.,0.,0.));
#13508=DIRECTION('center_axis',(0.,1.,0.));
#13509=DIRECTION('ref_axis',(1.,0.,0.));
#13510=DIRECTION('center_axis',(0.,1.,0.));
#13511=DIRECTION('ref_axis',(1.,0.,0.));
#13512=DIRECTION('center_axis',(0.,1.,0.));
#13513=DIRECTION('ref_axis',(1.,0.,0.));
#13514=DIRECTION('center_axis',(0.,1.,0.));
#13515=DIRECTION('ref_axis',(1.,0.,0.));
#13516=DIRECTION('center_axis',(0.,-1.,0.));
#13517=DIRECTION('ref_axis',(1.,0.,0.));
#13518=DIRECTION('center_axis',(0.,1.,0.));
#13519=DIRECTION('ref_axis',(1.,0.,0.));
#13520=DIRECTION('',(0.,-1.,0.));
#13521=DIRECTION('center_axis',(0.,1.,0.));
#13522=DIRECTION('ref_axis',(1.,0.,0.));
#13523=DIRECTION('',(0.,-1.,0.));
#13524=DIRECTION('center_axis',(0.,1.,0.));
#13525=DIRECTION('ref_axis',(1.,0.,0.));
#13526=DIRECTION('center_axis',(0.,1.,0.));
#13527=DIRECTION('ref_axis',(1.,0.,0.));
#13528=DIRECTION('',(0.,-1.,0.));
#13529=DIRECTION('center_axis',(0.,1.,0.));
#13530=DIRECTION('ref_axis',(1.,0.,0.));
#13531=DIRECTION('axis',(0.,0.,1.));
#13532=DIRECTION('refdir',(1.,0.,0.));
#13533=DIRECTION('center_axis',(0.,0.,1.));
#13534=DIRECTION('ref_axis',(1.,0.,0.));
#13535=DIRECTION('',(0.,1.,0.));
#13536=DIRECTION('center_axis',(0.,0.,1.));
#13537=DIRECTION('ref_axis',(1.,0.,0.));
#13538=DIRECTION('center_axis',(0.,0.,1.));
#13539=DIRECTION('ref_axis',(1.,0.,0.));
#13540=DIRECTION('center_axis',(0.,0.,1.));
#13541=DIRECTION('ref_axis',(1.,0.,0.));
#13542=DIRECTION('',(0.,0.,1.));
#13543=DIRECTION('center_axis',(0.,0.,1.));
#13544=DIRECTION('ref_axis',(1.,0.,0.));
#13545=DIRECTION('center_axis',(0.,0.,1.));
#13546=DIRECTION('ref_axis',(1.,0.,0.));
#13547=DIRECTION('',(0.,-1.,0.));
#13548=DIRECTION('center_axis',(0.,1.,0.));
#13549=DIRECTION('ref_axis',(1.,0.,0.));
#13550=DIRECTION('center_axis',(0.,-1.,0.));
#13551=DIRECTION('ref_axis',(1.,0.,0.));
#13552=DIRECTION('',(0.,-1.,0.));
#13553=DIRECTION('center_axis',(0.,-1.,0.));
#13554=DIRECTION('ref_axis',(1.,0.,0.));
#13555=DIRECTION('center_axis',(0.,1.,0.));
#13556=DIRECTION('ref_axis',(1.,0.,0.));
#13557=DIRECTION('center_axis',(0.,1.,0.));
#13558=DIRECTION('ref_axis',(1.,0.,0.));
#13559=DIRECTION('',(0.,-1.,0.));
#13560=DIRECTION('center_axis',(0.,1.,0.));
#13561=DIRECTION('ref_axis',(1.,0.,0.));
#13562=DIRECTION('center_axis',(0.,1.,0.));
#13563=DIRECTION('ref_axis',(1.,0.,0.));
#13564=DIRECTION('center_axis',(0.,1.,0.));
#13565=DIRECTION('ref_axis',(1.,0.,0.));
#13566=DIRECTION('axis',(0.,0.,1.));
#13567=DIRECTION('refdir',(1.,0.,0.));
#13568=DIRECTION('center_axis',(0.,0.,1.));
#13569=DIRECTION('ref_axis',(1.,0.,0.));
#13570=DIRECTION('',(0.,1.,0.));
#13571=DIRECTION('center_axis',(0.,0.,1.));
#13572=DIRECTION('ref_axis',(1.,0.,0.));
#13573=DIRECTION('center_axis',(0.,0.,1.));
#13574=DIRECTION('ref_axis',(1.,0.,0.));
#13575=DIRECTION('center_axis',(0.,0.,1.));
#13576=DIRECTION('ref_axis',(1.,0.,0.));
#13577=DIRECTION('',(0.,0.,1.));
#13578=DIRECTION('center_axis',(0.,0.,1.));
#13579=DIRECTION('ref_axis',(1.,0.,0.));
#13580=DIRECTION('center_axis',(0.,0.,1.));
#13581=DIRECTION('ref_axis',(1.,0.,0.));
#13582=DIRECTION('',(0.,-1.,0.));
#13583=DIRECTION('center_axis',(0.,1.,0.));
#13584=DIRECTION('ref_axis',(1.,0.,0.));
#13585=DIRECTION('center_axis',(0.,-1.,0.));
#13586=DIRECTION('ref_axis',(1.,0.,0.));
#13587=DIRECTION('',(0.,-1.,0.));
#13588=DIRECTION('center_axis',(0.,-1.,0.));
#13589=DIRECTION('ref_axis',(1.,0.,0.));
#13590=DIRECTION('center_axis',(0.,1.,0.));
#13591=DIRECTION('ref_axis',(1.,0.,0.));
#13592=DIRECTION('center_axis',(0.,1.,0.));
#13593=DIRECTION('ref_axis',(1.,0.,0.));
#13594=DIRECTION('',(0.,-1.,0.));
#13595=DIRECTION('center_axis',(0.,1.,0.));
#13596=DIRECTION('ref_axis',(1.,0.,0.));
#13597=DIRECTION('center_axis',(0.,1.,0.));
#13598=DIRECTION('ref_axis',(1.,0.,0.));
#13599=DIRECTION('center_axis',(0.,1.,0.));
#13600=DIRECTION('ref_axis',(1.,0.,0.));
#13601=DIRECTION('axis',(0.,0.,1.));
#13602=DIRECTION('refdir',(1.,0.,0.));
#13603=DIRECTION('center_axis',(0.,1.,0.));
#13604=DIRECTION('ref_axis',(1.,0.,0.));
#13605=DIRECTION('center_axis',(0.,-1.,0.));
#13606=DIRECTION('ref_axis',(1.,0.,0.));
#13607=DIRECTION('',(0.,-1.,0.));
#13608=DIRECTION('center_axis',(0.,-1.,0.));
#13609=DIRECTION('ref_axis',(1.,0.,0.));
#13610=DIRECTION('center_axis',(0.,1.,0.));
#13611=DIRECTION('ref_axis',(1.,0.,0.));
#13612=DIRECTION('center_axis',(0.,1.,0.));
#13613=DIRECTION('ref_axis',(1.,0.,0.));
#13614=DIRECTION('',(0.,-1.,0.));
#13615=DIRECTION('center_axis',(0.,1.,0.));
#13616=DIRECTION('ref_axis',(1.,0.,0.));
#13617=DIRECTION('center_axis',(0.,1.,0.));
#13618=DIRECTION('ref_axis',(1.,0.,0.));
#13619=DIRECTION('center_axis',(0.,1.,0.));
#13620=DIRECTION('ref_axis',(1.,0.,0.));
#13621=DIRECTION('axis',(0.,0.,1.));
#13622=DIRECTION('refdir',(1.,0.,0.));
#13623=DIRECTION('center_axis',(0.866025403784439,0.,-0.5));
#13624=DIRECTION('ref_axis',(0.5,0.,0.866025403784439));
#13625=DIRECTION('',(0.5,0.,0.866025403784439));
#13626=DIRECTION('',(0.,-1.,0.));
#13627=DIRECTION('',(0.5,0.,0.866025403784439));
#13628=DIRECTION('',(0.,-1.,0.));
#13629=DIRECTION('center_axis',(1.20185167898973E-16,0.,-1.));
#13630=DIRECTION('ref_axis',(1.,0.,1.20185167898973E-16));
#13631=DIRECTION('',(1.,0.,1.20185167898973E-16));
#13632=DIRECTION('',(0.,-1.,0.));
#13633=DIRECTION('',(1.,0.,1.20185167898973E-16));
#13634=DIRECTION('center_axis',(-0.866025403784439,0.,-0.5));
#13635=DIRECTION('ref_axis',(0.5,0.,-0.866025403784439));
#13636=DIRECTION('',(0.5,0.,-0.866025403784439));
#13637=DIRECTION('',(0.,-1.,0.));
#13638=DIRECTION('',(0.5,0.,-0.866025403784439));
#13639=DIRECTION('center_axis',(-0.866025403784439,0.,0.5));
#13640=DIRECTION('ref_axis',(-0.5,0.,-0.866025403784439));
#13641=DIRECTION('',(-0.5,0.,-0.866025403784439));
#13642=DIRECTION('',(0.,-1.,0.));
#13643=DIRECTION('',(-0.5,0.,-0.866025403784439));
#13644=DIRECTION('center_axis',(-2.40370335797945E-16,0.,1.));
#13645=DIRECTION('ref_axis',(-1.,0.,-2.40370335797945E-16));
#13646=DIRECTION('',(-1.,0.,-2.40370335797945E-16));
#13647=DIRECTION('',(0.,-1.,0.));
#13648=DIRECTION('',(-1.,0.,-2.40370335797945E-16));
#13649=DIRECTION('center_axis',(0.866025403784439,0.,0.5));
#13650=DIRECTION('ref_axis',(-0.5,0.,0.866025403784439));
#13651=DIRECTION('',(-0.5,0.,0.866025403784439));
#13652=DIRECTION('',(-0.5,0.,0.866025403784439));
#13653=DIRECTION('center_axis',(0.,-1.,0.));
#13654=DIRECTION('ref_axis',(0.,0.,-1.));
#13655=DIRECTION('center_axis',(0.,1.,0.));
#13656=DIRECTION('ref_axis',(0.,0.,1.));
#13657=DIRECTION('center_axis',(0.,-1.,0.));
#13658=DIRECTION('ref_axis',(1.,0.,0.));
#13659=DIRECTION('center_axis',(0.,-1.,0.));
#13660=DIRECTION('ref_axis',(1.,0.,0.));
#13661=DIRECTION('center_axis',(0.,-1.,0.));
#13662=DIRECTION('ref_axis',(1.,0.,0.));
#13663=DIRECTION('',(0.707106781186548,0.707106781186547,8.65956056235494E-17));
#13664=DIRECTION('center_axis',(0.,-1.,0.));
#13665=DIRECTION('ref_axis',(1.,0.,0.));
#13666=DIRECTION('center_axis',(0.,1.,0.));
#13667=DIRECTION('ref_axis',(1.,0.,0.));
#13668=DIRECTION('',(0.,1.,0.));
#13669=DIRECTION('center_axis',(0.,1.,0.));
#13670=DIRECTION('ref_axis',(1.,0.,0.));
#13671=DIRECTION('center_axis',(0.,-1.,0.));
#13672=DIRECTION('ref_axis',(1.,0.,0.));
#13673=DIRECTION('',(-0.707106781186548,0.707106781186547,-8.65956056235494E-17));
#13674=DIRECTION('center_axis',(0.,-1.,0.));
#13675=DIRECTION('ref_axis',(0.,0.,-1.));
#13676=DIRECTION('axis',(0.,0.,1.));
#13677=DIRECTION('refdir',(1.,0.,0.));
#13678=DIRECTION('axis',(0.,0.,1.));
#13679=DIRECTION('refdir',(1.,0.,0.));
#13680=DIRECTION('center_axis',(0.,0.,1.));
#13681=DIRECTION('ref_axis',(1.,0.,0.));
#13682=DIRECTION('',(0.,0.,1.));
#13683=DIRECTION('center_axis',(0.,1.,0.));
#13684=DIRECTION('ref_axis',(1.,0.,0.));
#13685=DIRECTION('center_axis',(0.,1.,0.));
#13686=DIRECTION('ref_axis',(1.,0.,0.));
#13687=DIRECTION('',(0.,1.,0.));
#13688=DIRECTION('center_axis',(0.,-1.,0.));
#13689=DIRECTION('ref_axis',(1.,0.,0.));
#13690=DIRECTION('center_axis',(-0.762527203906389,0.,0.646956152534856));
#13691=DIRECTION('ref_axis',(-0.646956152534856,0.,-0.762527203906389));
#13692=DIRECTION('',(0.646956152534856,0.,0.762527203906389));
#13693=DIRECTION('',(0.,-1.,0.));
#13694=DIRECTION('',(-0.646956152534856,0.,-0.762527203906389));
#13695=DIRECTION('',(0.,-1.,0.));
#13696=DIRECTION('center_axis',(-0.695442635009613,0.,0.718581617779697));
#13697=DIRECTION('ref_axis',(-0.718581617779697,0.,-0.695442635009613));
#13698=DIRECTION('',(0.718581617779697,0.,0.695442635009613));
#13699=DIRECTION('',(-0.718581617779697,0.,-0.695442635009613));
#13700=DIRECTION('',(0.,-1.,0.));
#13701=DIRECTION('center_axis',(-0.621660573370079,0.,0.783286749228649));
#13702=DIRECTION('ref_axis',(-0.783286749228649,0.,-0.621660573370079));
#13703=DIRECTION('',(0.783286749228649,0.,0.621660573370079));
#13704=DIRECTION('',(-0.783286749228649,0.,-0.621660573370079));
#13705=DIRECTION('',(0.,-1.,0.));
#13706=DIRECTION('center_axis',(-0.541891580574751,0.,0.840448401094439));
#13707=DIRECTION('ref_axis',(-0.840448401094439,0.,-0.541891580574751));
#13708=DIRECTION('',(0.840448401094439,0.,0.541891580574751));
#13709=DIRECTION('',(-0.840448401094439,0.,-0.541891580574751));
#13710=DIRECTION('',(0.,-1.,0.));
#13711=DIRECTION('center_axis',(-0.456903875630423,0.,0.889516075421855));
#13712=DIRECTION('ref_axis',(-0.889516075421855,0.,-0.456903875630423));
#13713=DIRECTION('',(0.889516075421855,0.,0.456903875630423));
#13714=DIRECTION('',(-0.889516075421855,0.,-0.456903875630423));
#13715=DIRECTION('',(0.,-1.,0.));
#13716=DIRECTION('center_axis',(-0.367515936594703,0.,0.930017223684012));
#13717=DIRECTION('ref_axis',(-0.930017223684012,0.,-0.367515936594703));
#13718=DIRECTION('',(0.930017223684012,0.,0.367515936594703));
#13719=DIRECTION('',(-0.930017223684012,0.,-0.367515936594703));
#13720=DIRECTION('',(0.,-1.,0.));
#13721=DIRECTION('center_axis',(-0.274588618184932,0.,0.961561797682962));
#13722=DIRECTION('ref_axis',(-0.961561797682962,0.,-0.274588618184932));
#13723=DIRECTION('',(0.961561797682962,0.,0.274588618184932));
#13724=DIRECTION('',(-0.961561797682962,0.,-0.274588618184932));
#13725=DIRECTION('',(0.,-1.,0.));
#13726=DIRECTION('center_axis',(-0.179016861276632,0.,0.983846005927077));
#13727=DIRECTION('ref_axis',(-0.983846005927077,0.,-0.179016861276632));
#13728=DIRECTION('',(0.983846005927077,0.,0.179016861276632));
#13729=DIRECTION('',(-0.983846005927077,0.,-0.179016861276632));
#13730=DIRECTION('',(0.,-1.,0.));
#13731=DIRECTION('center_axis',(0.99144486137381,0.,0.130526192220052));
#13732=DIRECTION('ref_axis',(-0.130526192220052,0.,0.99144486137381));
#13733=DIRECTION('',(0.130526192220052,0.,-0.99144486137381));
#13734=DIRECTION('',(-0.130526192220052,0.,0.99144486137381));
#13735=DIRECTION('',(0.,-1.,0.));
#13736=DIRECTION('center_axis',(0.179016861276633,0.,-0.983846005927077));
#13737=DIRECTION('ref_axis',(0.983846005927077,0.,0.179016861276633));
#13738=DIRECTION('',(-0.983846005927077,0.,-0.179016861276633));
#13739=DIRECTION('',(0.983846005927077,0.,0.179016861276633));
#13740=DIRECTION('',(0.,-1.,0.));
#13741=DIRECTION('center_axis',(0.274588618184932,0.,-0.961561797682962));
#13742=DIRECTION('ref_axis',(0.961561797682962,0.,0.274588618184932));
#13743=DIRECTION('',(-0.961561797682962,0.,-0.274588618184932));
#13744=DIRECTION('',(0.961561797682962,0.,0.274588618184932));
#13745=DIRECTION('',(0.,-1.,0.));
#13746=DIRECTION('center_axis',(0.367515936594704,0.,-0.930017223684012));
#13747=DIRECTION('ref_axis',(0.930017223684012,0.,0.367515936594704));
#13748=DIRECTION('',(-0.930017223684012,0.,-0.367515936594704));
#13749=DIRECTION('',(0.930017223684012,0.,0.367515936594704));
#13750=DIRECTION('',(0.,-1.,0.));
#13751=DIRECTION('center_axis',(0.456903875630421,0.,-0.889516075421856));
#13752=DIRECTION('ref_axis',(0.889516075421856,0.,0.456903875630421));
#13753=DIRECTION('',(-0.889516075421856,0.,-0.456903875630421));
#13754=DIRECTION('',(0.889516075421856,0.,0.456903875630421));
#13755=DIRECTION('',(0.,-1.,0.));
#13756=DIRECTION('center_axis',(0.541891580574752,0.,-0.840448401094438));
#13757=DIRECTION('ref_axis',(0.840448401094438,0.,0.541891580574752));
#13758=DIRECTION('',(-0.840448401094438,0.,-0.541891580574752));
#13759=DIRECTION('',(0.840448401094438,0.,0.541891580574752));
#13760=DIRECTION('',(0.,-1.,0.));
#13761=DIRECTION('center_axis',(0.621660573370078,0.,-0.78328674922865));
#13762=DIRECTION('ref_axis',(0.78328674922865,0.,0.621660573370078));
#13763=DIRECTION('',(-0.78328674922865,0.,-0.621660573370078));
#13764=DIRECTION('',(0.78328674922865,0.,0.621660573370078));
#13765=DIRECTION('',(0.,-1.,0.));
#13766=DIRECTION('center_axis',(0.695442635009612,0.,-0.718581617779697));
#13767=DIRECTION('ref_axis',(0.718581617779697,0.,0.695442635009612));
#13768=DIRECTION('',(-0.718581617779697,0.,-0.695442635009612));
#13769=DIRECTION('',(0.718581617779697,0.,0.695442635009612));
#13770=DIRECTION('',(0.,-1.,0.));
#13771=DIRECTION('center_axis',(0.762527203906389,0.,-0.646956152534857));
#13772=DIRECTION('ref_axis',(0.646956152534857,0.,0.762527203906389));
#13773=DIRECTION('',(-0.646956152534857,0.,-0.762527203906389));
#13774=DIRECTION('',(0.646956152534857,0.,0.762527203906389));
#13775=DIRECTION('',(0.,-1.,0.));
#13776=DIRECTION('center_axis',(-0.60876142900872,0.,-0.793353340291236));
#13777=DIRECTION('ref_axis',(0.793353340291236,0.,-0.60876142900872));
#13778=DIRECTION('',(-0.793353340291236,0.,0.60876142900872));
#13779=DIRECTION('',(0.793353340291236,0.,-0.60876142900872));
#13780=DIRECTION('center_axis',(0.,1.,0.));
#13781=DIRECTION('ref_axis',(-0.5,0.,0.866025403784438));
#13782=DIRECTION('center_axis',(0.,1.,0.));
#13783=DIRECTION('ref_axis',(1.,0.,0.));
#13784=DIRECTION('center_axis',(0.,1.,0.));
#13785=DIRECTION('ref_axis',(1.,0.,0.));
#13786=DIRECTION('center_axis',(0.,1.,0.));
#13787=DIRECTION('ref_axis',(1.,0.,0.));
#13788=DIRECTION('center_axis',(0.,1.,0.));
#13789=DIRECTION('ref_axis',(1.,0.,0.));
#13790=DIRECTION('center_axis',(0.,1.,0.));
#13791=DIRECTION('ref_axis',(1.,0.,0.));
#13792=DIRECTION('center_axis',(0.,1.,0.));
#13793=DIRECTION('ref_axis',(1.,0.,0.));
#13794=DIRECTION('center_axis',(0.,1.,0.));
#13795=DIRECTION('ref_axis',(1.,0.,0.));
#13796=DIRECTION('center_axis',(0.,1.,0.));
#13797=DIRECTION('ref_axis',(1.,0.,0.));
#13798=DIRECTION('center_axis',(0.,1.,0.));
#13799=DIRECTION('ref_axis',(1.,0.,0.));
#13800=DIRECTION('center_axis',(0.,1.,0.));
#13801=DIRECTION('ref_axis',(1.,0.,0.));
#13802=DIRECTION('center_axis',(0.,1.,0.));
#13803=DIRECTION('ref_axis',(1.,0.,0.));
#13804=DIRECTION('center_axis',(0.,1.,0.));
#13805=DIRECTION('ref_axis',(1.,0.,0.));
#13806=DIRECTION('center_axis',(0.,1.,0.));
#13807=DIRECTION('ref_axis',(1.,0.,0.));
#13808=DIRECTION('center_axis',(0.,1.,0.));
#13809=DIRECTION('ref_axis',(1.,0.,0.));
#13810=DIRECTION('center_axis',(0.,1.,0.));
#13811=DIRECTION('ref_axis',(1.,0.,0.));
#13812=DIRECTION('center_axis',(0.,1.,0.));
#13813=DIRECTION('ref_axis',(1.,0.,0.));
#13814=DIRECTION('center_axis',(0.,1.,0.));
#13815=DIRECTION('ref_axis',(1.,0.,0.));
#13816=DIRECTION('center_axis',(0.,1.,0.));
#13817=DIRECTION('ref_axis',(1.,0.,0.));
#13818=DIRECTION('',(-0.923879532511287,0.,-0.38268343236509));
#13819=DIRECTION('',(0.336889853392221,0.,-0.941544065183021));
#13820=DIRECTION('',(0.242980179903264,0.,-0.970031253194544));
#13821=DIRECTION('',(0.146730474455362,0.,-0.989176509964781));
#13822=DIRECTION('',(0.0490676743274181,0.,-0.998795456205172));
#13823=DIRECTION('',(-0.0490676743274181,0.,-0.998795456205172));
#13824=DIRECTION('',(-0.146730474455362,0.,-0.989176509964781));
#13825=DIRECTION('',(-0.242980179903264,0.,-0.970031253194544));
#13826=DIRECTION('',(-0.336889853392221,0.,-0.941544065183021));
#13827=DIRECTION('',(0.923879532511287,0.,-0.38268343236509));
#13828=DIRECTION('center_axis',(0.,1.,0.));
#13829=DIRECTION('ref_axis',(1.,0.,0.));
#13830=DIRECTION('',(0.130526192220051,0.,0.99144486137381));
#13831=DIRECTION('',(-0.983846005927078,0.,0.179016861276632));
#13832=DIRECTION('',(-0.961561797682962,0.,0.274588618184932));
#13833=DIRECTION('',(-0.930017223684012,0.,0.367515936594703));
#13834=DIRECTION('',(-0.889516075421856,0.,0.45690387563042));
#13835=DIRECTION('',(-0.840448401094438,0.,0.541891580574752));
#13836=DIRECTION('',(-0.78328674922865,0.,0.621660573370077));
#13837=DIRECTION('',(-0.718581617779698,0.,0.695442635009612));
#13838=DIRECTION('',(-0.646956152534857,0.,0.762527203906388));
#13839=DIRECTION('',(-0.793353340291235,0.,-0.608761429008721));
#13840=DIRECTION('center_axis',(0.,1.,0.));
#13841=DIRECTION('ref_axis',(1.,0.,0.));
#13842=DIRECTION('center_axis',(0.,1.,0.));
#13843=DIRECTION('ref_axis',(1.,0.,0.));
#13844=DIRECTION('center_axis',(-0.179016861276632,0.,-0.983846005927078));
#13845=DIRECTION('ref_axis',(0.983846005927078,0.,-0.179016861276632));
#13846=DIRECTION('',(-0.983846005927078,0.,0.179016861276632));
#13847=DIRECTION('',(0.,-1.,0.));
#13848=DIRECTION('',(0.983846005927078,0.,-0.179016861276632));
#13849=DIRECTION('',(0.,-1.,0.));
#13850=DIRECTION('center_axis',(-0.274588618184931,0.,-0.961561797682962));
#13851=DIRECTION('ref_axis',(0.961561797682962,0.,-0.274588618184931));
#13852=DIRECTION('',(-0.961561797682962,0.,0.274588618184931));
#13853=DIRECTION('',(0.961561797682962,0.,-0.274588618184931));
#13854=DIRECTION('',(0.,-1.,0.));
#13855=DIRECTION('center_axis',(-0.367515936594702,0.,-0.930017223684013));
#13856=DIRECTION('ref_axis',(0.930017223684013,0.,-0.367515936594702));
#13857=DIRECTION('',(-0.930017223684013,0.,0.367515936594703));
#13858=DIRECTION('',(0.930017223684013,0.,-0.367515936594702));
#13859=DIRECTION('',(0.,-1.,0.));
#13860=DIRECTION('center_axis',(-0.456903875630422,0.,-0.889516075421855));
#13861=DIRECTION('ref_axis',(0.889516075421855,0.,-0.456903875630422));
#13862=DIRECTION('',(-0.889516075421855,0.,0.456903875630422));
#13863=DIRECTION('',(0.889516075421855,0.,-0.456903875630422));
#13864=DIRECTION('',(0.,-1.,0.));
#13865=DIRECTION('center_axis',(-0.54189158057475,0.,-0.840448401094439));
#13866=DIRECTION('ref_axis',(0.840448401094439,0.,-0.54189158057475));
#13867=DIRECTION('',(-0.840448401094439,0.,0.54189158057475));
#13868=DIRECTION('',(0.840448401094439,0.,-0.54189158057475));
#13869=DIRECTION('',(0.,-1.,0.));
#13870=DIRECTION('center_axis',(-0.621660573370078,0.,-0.78328674922865));
#13871=DIRECTION('ref_axis',(0.78328674922865,0.,-0.621660573370078));
#13872=DIRECTION('',(-0.78328674922865,0.,0.621660573370078));
#13873=DIRECTION('',(0.78328674922865,0.,-0.621660573370078));
#13874=DIRECTION('',(0.,-1.,0.));
#13875=DIRECTION('center_axis',(-0.695442635009612,0.,-0.718581617779698));
#13876=DIRECTION('ref_axis',(0.718581617779698,0.,-0.695442635009612));
#13877=DIRECTION('',(-0.718581617779698,0.,0.695442635009612));
#13878=DIRECTION('',(0.718581617779698,0.,-0.695442635009612));
#13879=DIRECTION('',(0.,-1.,0.));
#13880=DIRECTION('center_axis',(-0.762527203906389,0.,-0.646956152534857));
#13881=DIRECTION('ref_axis',(0.646956152534857,0.,-0.762527203906389));
#13882=DIRECTION('',(-0.646956152534857,0.,0.762527203906389));
#13883=DIRECTION('',(0.646956152534857,0.,-0.762527203906389));
#13884=DIRECTION('',(0.,-1.,0.));
#13885=DIRECTION('center_axis',(-0.608761429008721,0.,0.793353340291235));
#13886=DIRECTION('ref_axis',(-0.793353340291235,0.,-0.608761429008721));
#13887=DIRECTION('',(0.793353340291235,0.,0.608761429008721));
#13888=DIRECTION('',(0.,-1.,0.));
#13889=DIRECTION('center_axis',(0.762527203906388,0.,0.646956152534857));
#13890=DIRECTION('ref_axis',(-0.646956152534857,0.,0.762527203906388));
#13891=DIRECTION('',(0.646956152534857,0.,-0.762527203906388));
#13892=DIRECTION('',(0.,-1.,0.));
#13893=DIRECTION('center_axis',(0.695442635009612,0.,0.718581617779698));
#13894=DIRECTION('ref_axis',(-0.718581617779698,0.,0.695442635009612));
#13895=DIRECTION('',(0.718581617779698,0.,-0.695442635009612));
#13896=DIRECTION('',(0.,-1.,0.));
#13897=DIRECTION('center_axis',(0.621660573370077,0.,0.78328674922865));
#13898=DIRECTION('ref_axis',(-0.78328674922865,0.,0.621660573370077));
#13899=DIRECTION('',(0.78328674922865,0.,-0.621660573370077));
#13900=DIRECTION('',(0.,-1.,0.));
#13901=DIRECTION('center_axis',(0.541891580574752,0.,0.840448401094438));
#13902=DIRECTION('ref_axis',(-0.840448401094438,0.,0.541891580574752));
#13903=DIRECTION('',(0.840448401094438,0.,-0.541891580574752));
#13904=DIRECTION('',(0.,-1.,0.));
#13905=DIRECTION('center_axis',(0.45690387563042,0.,0.889516075421856));
#13906=DIRECTION('ref_axis',(-0.889516075421856,0.,0.45690387563042));
#13907=DIRECTION('',(0.889516075421856,0.,-0.45690387563042));
#13908=DIRECTION('',(0.,-1.,0.));
#13909=DIRECTION('center_axis',(0.367515936594703,0.,0.930017223684012));
#13910=DIRECTION('ref_axis',(-0.930017223684012,0.,0.367515936594703));
#13911=DIRECTION('',(0.930017223684012,0.,-0.367515936594703));
#13912=DIRECTION('',(0.,-1.,0.));
#13913=DIRECTION('center_axis',(0.274588618184932,0.,0.961561797682962));
#13914=DIRECTION('ref_axis',(-0.961561797682962,0.,0.274588618184932));
#13915=DIRECTION('',(0.961561797682962,0.,-0.274588618184932));
#13916=DIRECTION('',(0.,-1.,0.));
#13917=DIRECTION('center_axis',(0.179016861276632,0.,0.983846005927078));
#13918=DIRECTION('ref_axis',(-0.983846005927078,0.,0.179016861276632));
#13919=DIRECTION('',(0.983846005927078,0.,-0.179016861276632));
#13920=DIRECTION('',(0.,-1.,0.));
#13921=DIRECTION('center_axis',(0.99144486137381,0.,-0.130526192220051));
#13922=DIRECTION('ref_axis',(0.130526192220051,0.,0.99144486137381));
#13923=DIRECTION('',(-0.130526192220051,0.,-0.99144486137381));
#13924=DIRECTION('center_axis',(0.,1.,0.));
#13925=DIRECTION('ref_axis',(-0.5,0.,-0.866025403784439));
#13926=DIRECTION('center_axis',(0.,1.,0.));
#13927=DIRECTION('ref_axis',(1.,0.,0.));
#13928=DIRECTION('center_axis',(0.,1.,0.));
#13929=DIRECTION('ref_axis',(1.,0.,0.));
#13930=DIRECTION('center_axis',(0.,1.,0.));
#13931=DIRECTION('ref_axis',(1.,0.,0.));
#13932=DIRECTION('center_axis',(0.,1.,0.));
#13933=DIRECTION('ref_axis',(1.,0.,0.));
#13934=DIRECTION('center_axis',(0.,1.,0.));
#13935=DIRECTION('ref_axis',(1.,0.,0.));
#13936=DIRECTION('center_axis',(0.,1.,0.));
#13937=DIRECTION('ref_axis',(1.,0.,0.));
#13938=DIRECTION('center_axis',(0.,1.,0.));
#13939=DIRECTION('ref_axis',(1.,0.,0.));
#13940=DIRECTION('center_axis',(0.,1.,0.));
#13941=DIRECTION('ref_axis',(1.,0.,0.));
#13942=DIRECTION('center_axis',(0.,1.,0.));
#13943=DIRECTION('ref_axis',(1.,0.,0.));
#13944=DIRECTION('center_axis',(0.,1.,0.));
#13945=DIRECTION('ref_axis',(1.,0.,0.));
#13946=DIRECTION('center_axis',(0.,1.,0.));
#13947=DIRECTION('ref_axis',(1.,0.,0.));
#13948=DIRECTION('center_axis',(0.,1.,0.));
#13949=DIRECTION('ref_axis',(1.,0.,0.));
#13950=DIRECTION('center_axis',(0.,1.,0.));
#13951=DIRECTION('ref_axis',(1.,0.,0.));
#13952=DIRECTION('center_axis',(0.,1.,0.));
#13953=DIRECTION('ref_axis',(1.,0.,0.));
#13954=DIRECTION('center_axis',(0.,1.,0.));
#13955=DIRECTION('ref_axis',(1.,0.,0.));
#13956=DIRECTION('center_axis',(0.,1.,0.));
#13957=DIRECTION('ref_axis',(1.,0.,0.));
#13958=DIRECTION('center_axis',(0.94154406518302,0.,0.336889853392221));
#13959=DIRECTION('ref_axis',(-0.336889853392221,0.,0.94154406518302));
#13960=DIRECTION('',(0.336889853392221,0.,-0.94154406518302));
#13961=DIRECTION('',(0.,-1.,0.));
#13962=DIRECTION('',(-0.336889853392221,0.,0.94154406518302));
#13963=DIRECTION('',(0.,-1.,0.));
#13964=DIRECTION('center_axis',(0.970031253194544,0.,0.242980179903265));
#13965=DIRECTION('ref_axis',(-0.242980179903265,0.,0.970031253194544));
#13966=DIRECTION('',(0.242980179903265,0.,-0.970031253194544));
#13967=DIRECTION('',(-0.242980179903265,0.,0.970031253194544));
#13968=DIRECTION('',(0.,-1.,0.));
#13969=DIRECTION('center_axis',(0.989176509964781,0.,0.146730474455363));
#13970=DIRECTION('ref_axis',(-0.146730474455363,0.,0.989176509964781));
#13971=DIRECTION('',(0.146730474455363,0.,-0.989176509964781));
#13972=DIRECTION('',(-0.146730474455363,0.,0.989176509964781));
#13973=DIRECTION('',(0.,-1.,0.));
#13974=DIRECTION('center_axis',(0.998795456205173,0.,0.049067674327416));
#13975=DIRECTION('ref_axis',(-0.049067674327416,0.,0.998795456205173));
#13976=DIRECTION('',(0.049067674327416,0.,-0.998795456205173));
#13977=DIRECTION('',(-0.049067674327416,0.,0.998795456205173));
#13978=DIRECTION('',(0.,-1.,0.));
#13979=DIRECTION('center_axis',(0.998795456205173,0.,-0.049067674327416));
#13980=DIRECTION('ref_axis',(0.049067674327416,0.,0.998795456205173));
#13981=DIRECTION('',(-0.049067674327416,0.,-0.998795456205173));
#13982=DIRECTION('',(0.049067674327416,0.,0.998795456205173));
#13983=DIRECTION('',(0.,-1.,0.));
#13984=DIRECTION('center_axis',(0.989176509964781,0.,-0.146730474455363));
#13985=DIRECTION('ref_axis',(0.146730474455363,0.,0.989176509964781));
#13986=DIRECTION('',(-0.146730474455363,0.,-0.989176509964781));
#13987=DIRECTION('',(0.146730474455363,0.,0.989176509964781));
#13988=DIRECTION('',(0.,-1.,0.));
#13989=DIRECTION('center_axis',(0.970031253194544,0.,-0.242980179903265));
#13990=DIRECTION('ref_axis',(0.242980179903265,0.,0.970031253194544));
#13991=DIRECTION('',(-0.242980179903265,0.,-0.970031253194544));
#13992=DIRECTION('',(0.242980179903265,0.,0.970031253194544));
#13993=DIRECTION('',(0.,-1.,0.));
#13994=DIRECTION('center_axis',(0.94154406518302,0.,-0.336889853392221));
#13995=DIRECTION('ref_axis',(0.336889853392221,0.,0.94154406518302));
#13996=DIRECTION('',(-0.336889853392221,0.,-0.94154406518302));
#13997=DIRECTION('',(0.336889853392221,0.,0.94154406518302));
#13998=DIRECTION('',(0.,-1.,0.));
#13999=DIRECTION('center_axis',(-0.38268343236509,0.,-0.923879532511287));
#14000=DIRECTION('ref_axis',(0.923879532511287,0.,-0.38268343236509));
#14001=DIRECTION('',(-0.923879532511287,0.,0.38268343236509));
#14002=DIRECTION('',(0.,-1.,0.));
#14003=DIRECTION('center_axis',(-0.941544065183021,0.,0.336889853392221));
#14004=DIRECTION('ref_axis',(-0.336889853392221,0.,-0.941544065183021));
#14005=DIRECTION('',(0.336889853392221,0.,0.941544065183021));
#14006=DIRECTION('',(0.,-1.,0.));
#14007=DIRECTION('center_axis',(-0.970031253194544,0.,0.242980179903264));
#14008=DIRECTION('ref_axis',(-0.242980179903264,0.,-0.970031253194544));
#14009=DIRECTION('',(0.242980179903264,0.,0.970031253194544));
#14010=DIRECTION('',(0.,-1.,0.));
#14011=DIRECTION('center_axis',(-0.989176509964781,0.,0.146730474455362));
#14012=DIRECTION('ref_axis',(-0.146730474455362,0.,-0.989176509964781));
#14013=DIRECTION('',(0.146730474455362,0.,0.989176509964781));
#14014=DIRECTION('',(0.,-1.,0.));
#14015=DIRECTION('center_axis',(-0.998795456205172,0.,0.0490676743274181));
#14016=DIRECTION('ref_axis',(-0.0490676743274181,0.,-0.998795456205172));
#14017=DIRECTION('',(0.0490676743274181,0.,0.998795456205172));
#14018=DIRECTION('',(0.,-1.,0.));
#14019=DIRECTION('center_axis',(-0.998795456205172,0.,-0.0490676743274181));
#14020=DIRECTION('ref_axis',(0.0490676743274181,0.,-0.998795456205172));
#14021=DIRECTION('',(-0.0490676743274181,0.,0.998795456205172));
#14022=DIRECTION('',(0.,-1.,0.));
#14023=DIRECTION('center_axis',(-0.989176509964781,0.,-0.146730474455362));
#14024=DIRECTION('ref_axis',(0.146730474455362,0.,-0.989176509964781));
#14025=DIRECTION('',(-0.146730474455362,0.,0.989176509964781));
#14026=DIRECTION('',(0.,-1.,0.));
#14027=DIRECTION('center_axis',(-0.970031253194544,0.,-0.242980179903264));
#14028=DIRECTION('ref_axis',(0.242980179903264,0.,-0.970031253194544));
#14029=DIRECTION('',(-0.242980179903264,0.,0.970031253194544));
#14030=DIRECTION('',(0.,-1.,0.));
#14031=DIRECTION('center_axis',(-0.941544065183021,0.,-0.336889853392221));
#14032=DIRECTION('ref_axis',(0.336889853392221,0.,-0.941544065183021));
#14033=DIRECTION('',(-0.336889853392221,0.,0.941544065183021));
#14034=DIRECTION('',(0.,-1.,0.));
#14035=DIRECTION('center_axis',(-0.38268343236509,0.,0.923879532511287));
#14036=DIRECTION('ref_axis',(-0.923879532511287,0.,-0.38268343236509));
#14037=DIRECTION('',(0.923879532511287,0.,0.38268343236509));
#14038=DIRECTION('center_axis',(0.,1.,0.));
#14039=DIRECTION('ref_axis',(1.,0.,0.));
#14040=DIRECTION('center_axis',(0.,1.,0.));
#14041=DIRECTION('ref_axis',(1.,0.,0.));
#14042=DIRECTION('center_axis',(0.,1.,0.));
#14043=DIRECTION('ref_axis',(1.,0.,0.));
#14044=DIRECTION('center_axis',(0.,1.,0.));
#14045=DIRECTION('ref_axis',(1.,0.,0.));
#14046=DIRECTION('center_axis',(0.,1.,0.));
#14047=DIRECTION('ref_axis',(1.,0.,0.));
#14048=DIRECTION('center_axis',(0.,1.,0.));
#14049=DIRECTION('ref_axis',(1.,0.,0.));
#14050=DIRECTION('center_axis',(0.,1.,0.));
#14051=DIRECTION('ref_axis',(1.,0.,0.));
#14052=DIRECTION('center_axis',(0.,1.,0.));
#14053=DIRECTION('ref_axis',(1.,0.,0.));
#14054=DIRECTION('center_axis',(0.,1.,0.));
#14055=DIRECTION('ref_axis',(1.,0.,0.));
#14056=DIRECTION('center_axis',(0.,1.,0.));
#14057=DIRECTION('ref_axis',(1.,0.,0.));
#14058=DIRECTION('center_axis',(0.,1.,0.));
#14059=DIRECTION('ref_axis',(1.,0.,0.));
#14060=DIRECTION('center_axis',(0.,1.,0.));
#14061=DIRECTION('ref_axis',(1.,0.,0.));
#14062=DIRECTION('center_axis',(0.,1.,0.));
#14063=DIRECTION('ref_axis',(1.,0.,0.));
#14064=DIRECTION('center_axis',(0.,1.,0.));
#14065=DIRECTION('ref_axis',(1.,0.,0.));
#14066=DIRECTION('center_axis',(0.,1.,0.));
#14067=DIRECTION('ref_axis',(1.,0.,0.));
#14068=DIRECTION('center_axis',(0.,1.,0.));
#14069=DIRECTION('ref_axis',(1.,0.,0.));
#14070=DIRECTION('center_axis',(0.,1.,0.));
#14071=DIRECTION('ref_axis',(1.,0.,0.));
#14072=DIRECTION('center_axis',(0.,-1.,0.));
#14073=DIRECTION('ref_axis',(1.,0.,0.));
#14074=DIRECTION('center_axis',(0.,-1.,0.));
#14075=DIRECTION('ref_axis',(1.,0.,0.));
#14076=DIRECTION('',(0.,1.,0.));
#14077=DIRECTION('center_axis',(0.,1.,0.));
#14078=DIRECTION('ref_axis',(1.,0.,0.));
#14079=DIRECTION('axis',(0.,0.,1.));
#14080=DIRECTION('refdir',(1.,0.,0.));
#14081=DIRECTION('center_axis',(0.866025403784439,0.,0.5));
#14082=DIRECTION('ref_axis',(0.5,0.,-0.866025403784439));
#14083=DIRECTION('',(0.866025403784439,0.,0.5));
#14084=DIRECTION('center_axis',(0.,1.,0.));
#14085=DIRECTION('ref_axis',(0.5,0.,-0.866025403784439));
#14086=DIRECTION('center_axis',(0.,1.,0.));
#14087=DIRECTION('ref_axis',(0.5,0.,-0.866025403784439));
#14088=DIRECTION('',(0.,1.,0.));
#14089=DIRECTION('center_axis',(0.,-1.,0.));
#14090=DIRECTION('ref_axis',(0.5,0.,-0.866025403784439));
#14091=DIRECTION('center_axis',(-0.179016861276632,0.,-0.983846005927078));
#14092=DIRECTION('ref_axis',(-0.983846005927078,0.,0.179016861276632));
#14093=DIRECTION('',(-0.983846005927078,0.,0.179016861276632));
#14094=DIRECTION('',(0.,1.,0.));
#14095=DIRECTION('',(-0.983846005927078,0.,0.179016861276632));
#14096=DIRECTION('',(0.,1.,0.));
#14097=DIRECTION('center_axis',(-0.274588618184931,0.,-0.961561797682962));
#14098=DIRECTION('ref_axis',(-0.961561797682962,0.,0.274588618184931));
#14099=DIRECTION('',(-0.961561797682962,0.,0.274588618184931));
#14100=DIRECTION('',(-0.961561797682962,0.,0.274588618184931));
#14101=DIRECTION('',(0.,1.,0.));
#14102=DIRECTION('center_axis',(-0.367515936594703,0.,-0.930017223684013));
#14103=DIRECTION('ref_axis',(-0.930017223684012,0.,0.367515936594703));
#14104=DIRECTION('',(-0.930017223684012,0.,0.367515936594703));
#14105=DIRECTION('',(-0.930017223684013,0.,0.367515936594703));
#14106=DIRECTION('',(0.,1.,0.));
#14107=DIRECTION('center_axis',(-0.45690387563042,0.,-0.889516075421857));
#14108=DIRECTION('ref_axis',(-0.889516075421857,0.,0.45690387563042));
#14109=DIRECTION('',(-0.889516075421857,0.,0.45690387563042));
#14110=DIRECTION('',(-0.889516075421857,0.,0.45690387563042));
#14111=DIRECTION('',(0.,1.,0.));
#14112=DIRECTION('center_axis',(-0.541891580574751,0.,-0.840448401094438));
#14113=DIRECTION('ref_axis',(-0.840448401094438,0.,0.541891580574751));
#14114=DIRECTION('',(-0.840448401094438,0.,0.541891580574751));
#14115=DIRECTION('',(-0.840448401094438,0.,0.541891580574751));
#14116=DIRECTION('',(0.,1.,0.));
#14117=DIRECTION('center_axis',(-0.621660573370077,0.,-0.783286749228651));
#14118=DIRECTION('ref_axis',(-0.783286749228651,0.,0.621660573370077));
#14119=DIRECTION('',(-0.783286749228651,0.,0.621660573370077));
#14120=DIRECTION('',(-0.783286749228651,0.,0.621660573370077));
#14121=DIRECTION('',(0.,1.,0.));
#14122=DIRECTION('center_axis',(-0.695442635009612,0.,-0.718581617779698));
#14123=DIRECTION('ref_axis',(-0.718581617779698,0.,0.695442635009612));
#14124=DIRECTION('',(-0.718581617779698,0.,0.695442635009612));
#14125=DIRECTION('',(-0.718581617779698,0.,0.695442635009612));
#14126=DIRECTION('',(0.,1.,0.));
#14127=DIRECTION('center_axis',(-0.762527203906388,0.,-0.646956152534857));
#14128=DIRECTION('ref_axis',(-0.646956152534857,0.,0.762527203906388));
#14129=DIRECTION('',(-0.646956152534858,0.,0.762527203906388));
#14130=DIRECTION('',(-0.646956152534857,0.,0.762527203906388));
#14131=DIRECTION('',(0.,1.,0.));
#14132=DIRECTION('center_axis',(0.608761429008721,0.,-0.793353340291235));
#14133=DIRECTION('ref_axis',(-0.793353340291235,0.,-0.608761429008721));
#14134=DIRECTION('',(-0.793353340291235,0.,-0.608761429008721));
#14135=DIRECTION('',(-0.793353340291235,0.,-0.608761429008721));
#14136=DIRECTION('',(0.,1.,0.));
#14137=DIRECTION('center_axis',(0.762527203906388,0.,0.646956152534857));
#14138=DIRECTION('ref_axis',(0.646956152534857,0.,-0.762527203906388));
#14139=DIRECTION('',(0.646956152534857,0.,-0.762527203906388));
#14140=DIRECTION('',(0.646956152534857,0.,-0.762527203906388));
#14141=DIRECTION('',(0.,1.,0.));
#14142=DIRECTION('center_axis',(0.695442635009612,0.,0.718581617779698));
#14143=DIRECTION('ref_axis',(0.718581617779698,0.,-0.695442635009612));
#14144=DIRECTION('',(0.718581617779698,0.,-0.695442635009612));
#14145=DIRECTION('',(0.718581617779698,0.,-0.695442635009612));
#14146=DIRECTION('',(0.,1.,0.));
#14147=DIRECTION('center_axis',(0.621660573370078,0.,0.78328674922865));
#14148=DIRECTION('ref_axis',(0.78328674922865,0.,-0.621660573370078));
#14149=DIRECTION('',(0.78328674922865,0.,-0.621660573370078));
#14150=DIRECTION('',(0.78328674922865,0.,-0.621660573370078));
#14151=DIRECTION('',(0.,1.,0.));
#14152=DIRECTION('center_axis',(0.54189158057475,0.,0.84044840109444));
#14153=DIRECTION('ref_axis',(0.84044840109444,0.,-0.54189158057475));
#14154=DIRECTION('',(0.84044840109444,0.,-0.54189158057475));
#14155=DIRECTION('',(0.84044840109444,0.,-0.54189158057475));
#14156=DIRECTION('',(0.,1.,0.));
#14157=DIRECTION('center_axis',(0.456903875630422,0.,0.889516075421856));
#14158=DIRECTION('ref_axis',(0.889516075421856,0.,-0.456903875630422));
#14159=DIRECTION('',(0.889516075421856,0.,-0.456903875630422));
#14160=DIRECTION('',(0.889516075421856,0.,-0.456903875630422));
#14161=DIRECTION('',(0.,1.,0.));
#14162=DIRECTION('center_axis',(0.367515936594702,0.,0.930017223684013));
#14163=DIRECTION('ref_axis',(0.930017223684013,0.,-0.367515936594702));
#14164=DIRECTION('',(0.930017223684013,0.,-0.367515936594702));
#14165=DIRECTION('',(0.930017223684013,0.,-0.367515936594702));
#14166=DIRECTION('',(0.,1.,0.));
#14167=DIRECTION('center_axis',(0.274588618184931,0.,0.961561797682962));
#14168=DIRECTION('ref_axis',(0.961561797682962,0.,-0.274588618184931));
#14169=DIRECTION('',(0.961561797682962,0.,-0.274588618184931));
#14170=DIRECTION('',(0.961561797682962,0.,-0.274588618184931));
#14171=DIRECTION('',(0.,1.,0.));
#14172=DIRECTION('center_axis',(0.179016861276631,0.,0.983846005927078));
#14173=DIRECTION('ref_axis',(0.983846005927078,0.,-0.179016861276631));
#14174=DIRECTION('',(0.983846005927078,0.,-0.179016861276631));
#14175=DIRECTION('',(0.983846005927078,0.,-0.179016861276631));
#14176=DIRECTION('',(0.,1.,0.));
#14177=DIRECTION('center_axis',(-0.99144486137381,0.,0.130526192220051));
#14178=DIRECTION('ref_axis',(0.130526192220051,0.,0.99144486137381));
#14179=DIRECTION('',(0.130526192220051,0.,0.99144486137381));
#14180=DIRECTION('',(0.130526192220051,0.,0.99144486137381));
#14181=DIRECTION('center_axis',(0.,1.,0.));
#14182=DIRECTION('ref_axis',(0.499999999999999,0.,0.866025403784439));
#14183=DIRECTION('center_axis',(0.,1.,0.));
#14184=DIRECTION('ref_axis',(0.5,0.,-0.866025403784439));
#14185=DIRECTION('center_axis',(0.,1.,0.));
#14186=DIRECTION('ref_axis',(0.5,0.,-0.866025403784438));
#14187=DIRECTION('center_axis',(0.,1.,0.));
#14188=DIRECTION('ref_axis',(0.5,0.,-0.866025403784439));
#14189=DIRECTION('center_axis',(0.,1.,0.));
#14190=DIRECTION('ref_axis',(0.5,0.,-0.866025403784438));
#14191=DIRECTION('center_axis',(0.,1.,0.));
#14192=DIRECTION('ref_axis',(0.5,0.,-0.866025403784439));
#14193=DIRECTION('center_axis',(0.,1.,0.));
#14194=DIRECTION('ref_axis',(0.5,0.,-0.866025403784438));
#14195=DIRECTION('center_axis',(0.,1.,0.));
#14196=DIRECTION('ref_axis',(0.5,0.,-0.866025403784439));
#14197=DIRECTION('center_axis',(0.,1.,0.));
#14198=DIRECTION('ref_axis',(0.5,0.,-0.866025403784438));
#14199=DIRECTION('center_axis',(0.,1.,0.));
#14200=DIRECTION('ref_axis',(0.5,0.,-0.866025403784439));
#14201=DIRECTION('center_axis',(0.,1.,0.));
#14202=DIRECTION('ref_axis',(0.5,0.,-0.866025403784438));
#14203=DIRECTION('center_axis',(0.,1.,0.));
#14204=DIRECTION('ref_axis',(0.5,0.,-0.866025403784439));
#14205=DIRECTION('center_axis',(0.,1.,0.));
#14206=DIRECTION('ref_axis',(0.5,0.,-0.866025403784438));
#14207=DIRECTION('center_axis',(0.,1.,0.));
#14208=DIRECTION('ref_axis',(0.5,0.,-0.866025403784439));
#14209=DIRECTION('center_axis',(0.,1.,0.));
#14210=DIRECTION('ref_axis',(0.5,0.,-0.866025403784438));
#14211=DIRECTION('center_axis',(0.,1.,0.));
#14212=DIRECTION('ref_axis',(0.5,0.,-0.866025403784438));
#14213=DIRECTION('',(0.923879532511287,0.,-0.38268343236509));
#14214=DIRECTION('',(-0.33688985339222,0.,-0.941544065183021));
#14215=DIRECTION('',(-0.242980179903264,0.,-0.970031253194544));
#14216=DIRECTION('',(-0.146730474455362,0.,-0.989176509964781));
#14217=DIRECTION('',(-0.0490676743274178,0.,-0.998795456205172));
#14218=DIRECTION('',(0.0490676743274185,0.,-0.998795456205172));
#14219=DIRECTION('',(0.146730474455362,0.,-0.989176509964781));
#14220=DIRECTION('',(0.242980179903265,0.,-0.970031253194544));
#14221=DIRECTION('',(0.336889853392221,0.,-0.941544065183021));
#14222=DIRECTION('',(-0.923879532511287,0.,-0.38268343236509));
#14223=DIRECTION('center_axis',(0.,1.,0.));
#14224=DIRECTION('ref_axis',(0.5,0.,-0.866025403784438));
#14225=DIRECTION('',(-0.130526192220052,0.,0.99144486137381));
#14226=DIRECTION('',(0.983846005927078,0.,0.179016861276632));
#14227=DIRECTION('',(0.961561797682962,0.,0.274588618184932));
#14228=DIRECTION('',(0.930017223684012,0.,0.367515936594704));
#14229=DIRECTION('',(0.889516075421856,0.,0.456903875630421));
#14230=DIRECTION('',(0.840448401094438,0.,0.541891580574752));
#14231=DIRECTION('',(0.78328674922865,0.,0.621660573370078));
#14232=DIRECTION('',(0.718581617779698,0.,0.695442635009612));
#14233=DIRECTION('',(0.646956152534857,0.,0.762527203906389));
#14234=DIRECTION('',(0.793353340291235,0.,-0.60876142900872));
#14235=DIRECTION('center_axis',(0.,1.,0.));
#14236=DIRECTION('ref_axis',(0.5,0.,-0.866025403784438));
#14237=DIRECTION('center_axis',(0.,1.,0.));
#14238=DIRECTION('ref_axis',(0.5,0.,-0.866025403784439));
#14239=DIRECTION('center_axis',(0.,1.,0.));
#14240=DIRECTION('ref_axis',(0.5,0.,-0.866025403784438));
#14241=DIRECTION('center_axis',(0.,1.,0.));
#14242=DIRECTION('ref_axis',(0.5,0.,-0.866025403784439));
#14243=DIRECTION('center_axis',(0.,1.,0.));
#14244=DIRECTION('ref_axis',(0.5,0.,-0.866025403784438));
#14245=DIRECTION('center_axis',(0.941544065183021,0.,0.336889853392221));
#14246=DIRECTION('ref_axis',(0.336889853392221,0.,-0.941544065183021));
#14247=DIRECTION('',(0.336889853392221,0.,-0.941544065183021));
#14248=DIRECTION('',(0.,1.,0.));
#14249=DIRECTION('',(0.,1.,0.));
#14250=DIRECTION('center_axis',(0.970031253194544,0.,0.242980179903265));
#14251=DIRECTION('ref_axis',(0.242980179903265,0.,-0.970031253194544));
#14252=DIRECTION('',(0.242980179903265,0.,-0.970031253194544));
#14253=DIRECTION('',(0.,1.,0.));
#14254=DIRECTION('center_axis',(0.989176509964781,0.,0.146730474455362));
#14255=DIRECTION('ref_axis',(0.146730474455362,0.,-0.989176509964781));
#14256=DIRECTION('',(0.146730474455362,0.,-0.989176509964781));
#14257=DIRECTION('',(0.,1.,0.));
#14258=DIRECTION('center_axis',(0.998795456205172,0.,0.0490676743274185));
#14259=DIRECTION('ref_axis',(0.0490676743274185,0.,-0.998795456205172));
#14260=DIRECTION('',(0.0490676743274185,0.,-0.998795456205172));
#14261=DIRECTION('',(0.,1.,0.));
#14262=DIRECTION('center_axis',(0.998795456205172,0.,-0.0490676743274178));
#14263=DIRECTION('ref_axis',(-0.0490676743274178,0.,-0.998795456205172));
#14264=DIRECTION('',(-0.0490676743274178,0.,-0.998795456205172));
#14265=DIRECTION('',(0.,1.,0.));
#14266=DIRECTION('center_axis',(0.989176509964781,0.,-0.146730474455361));
#14267=DIRECTION('ref_axis',(-0.146730474455361,0.,-0.989176509964781));
#14268=DIRECTION('',(-0.146730474455361,0.,-0.989176509964781));
#14269=DIRECTION('',(0.,1.,0.));
#14270=DIRECTION('center_axis',(0.970031253194544,0.,-0.242980179903264));
#14271=DIRECTION('ref_axis',(-0.242980179903264,0.,-0.970031253194544));
#14272=DIRECTION('',(-0.242980179903264,0.,-0.970031253194544));
#14273=DIRECTION('',(0.,1.,0.));
#14274=DIRECTION('center_axis',(0.941544065183021,0.,-0.33688985339222));
#14275=DIRECTION('ref_axis',(-0.33688985339222,0.,-0.941544065183021));
#14276=DIRECTION('',(-0.33688985339222,0.,-0.941544065183021));
#14277=DIRECTION('',(0.,1.,0.));
#14278=DIRECTION('center_axis',(0.38268343236509,0.,0.923879532511287));
#14279=DIRECTION('ref_axis',(0.923879532511287,0.,-0.38268343236509));
#14280=DIRECTION('',(0.923879532511287,0.,-0.38268343236509));
#14281=DIRECTION('',(0.,1.,0.));
#14282=DIRECTION('center_axis',(-0.941544065183021,0.,0.336889853392221));
#14283=DIRECTION('ref_axis',(0.336889853392221,0.,0.941544065183021));
#14284=DIRECTION('',(0.336889853392221,0.,0.941544065183021));
#14285=DIRECTION('',(0.336889853392221,0.,0.941544065183021));
#14286=DIRECTION('',(0.,1.,0.));
#14287=DIRECTION('center_axis',(-0.970031253194544,0.,0.242980179903264));
#14288=DIRECTION('ref_axis',(0.242980179903264,0.,0.970031253194544));
#14289=DIRECTION('',(0.242980179903264,0.,0.970031253194544));
#14290=DIRECTION('',(0.242980179903264,0.,0.970031253194544));
#14291=DIRECTION('',(0.,1.,0.));
#14292=DIRECTION('center_axis',(-0.989176509964781,0.,0.146730474455362));
#14293=DIRECTION('ref_axis',(0.146730474455362,0.,0.989176509964781));
#14294=DIRECTION('',(0.146730474455362,0.,0.989176509964781));
#14295=DIRECTION('',(0.146730474455362,0.,0.989176509964781));
#14296=DIRECTION('',(0.,1.,0.));
#14297=DIRECTION('center_axis',(-0.998795456205173,0.,0.0490676743274157));
#14298=DIRECTION('ref_axis',(0.0490676743274157,0.,0.998795456205173));
#14299=DIRECTION('',(0.0490676743274157,0.,0.998795456205173));
#14300=DIRECTION('',(0.0490676743274157,0.,0.998795456205173));
#14301=DIRECTION('',(0.,1.,0.));
#14302=DIRECTION('center_axis',(-0.998795456205173,0.,-0.0490676743274162));
#14303=DIRECTION('ref_axis',(-0.0490676743274162,0.,0.998795456205173));
#14304=DIRECTION('',(-0.0490676743274162,0.,0.998795456205173));
#14305=DIRECTION('',(-0.0490676743274162,0.,0.998795456205173));
#14306=DIRECTION('',(0.,1.,0.));
#14307=DIRECTION('center_axis',(-0.989176509964781,0.,-0.146730474455363));
#14308=DIRECTION('ref_axis',(-0.146730474455363,0.,0.989176509964781));
#14309=DIRECTION('',(-0.146730474455363,0.,0.989176509964781));
#14310=DIRECTION('',(-0.146730474455363,0.,0.989176509964781));
#14311=DIRECTION('',(0.,1.,0.));
#14312=DIRECTION('center_axis',(-0.970031253194544,0.,-0.242980179903265));
#14313=DIRECTION('ref_axis',(-0.242980179903265,0.,0.970031253194544));
#14314=DIRECTION('',(-0.242980179903265,0.,0.970031253194544));
#14315=DIRECTION('',(-0.242980179903265,0.,0.970031253194544));
#14316=DIRECTION('',(0.,1.,0.));
#14317=DIRECTION('center_axis',(-0.94154406518302,0.,-0.336889853392221));
#14318=DIRECTION('ref_axis',(-0.336889853392221,0.,0.94154406518302));
#14319=DIRECTION('',(-0.336889853392221,0.,0.94154406518302));
#14320=DIRECTION('',(-0.336889853392221,0.,0.94154406518302));
#14321=DIRECTION('',(0.,1.,0.));
#14322=DIRECTION('center_axis',(0.38268343236509,0.,-0.923879532511287));
#14323=DIRECTION('ref_axis',(-0.923879532511287,0.,-0.38268343236509));
#14324=DIRECTION('',(-0.923879532511287,0.,-0.38268343236509));
#14325=DIRECTION('center_axis',(0.,1.,0.));
#14326=DIRECTION('ref_axis',(-1.,0.,-3.33066907387547E-16));
#14327=DIRECTION('center_axis',(0.,1.,0.));
#14328=DIRECTION('ref_axis',(0.5,0.,-0.866025403784439));
#14329=DIRECTION('center_axis',(0.,1.,0.));
#14330=DIRECTION('ref_axis',(0.5,0.,-0.866025403784438));
#14331=DIRECTION('center_axis',(0.,1.,0.));
#14332=DIRECTION('ref_axis',(0.5,0.,-0.866025403784439));
#14333=DIRECTION('center_axis',(0.,1.,0.));
#14334=DIRECTION('ref_axis',(0.5,0.,-0.866025403784438));
#14335=DIRECTION('center_axis',(0.,1.,0.));
#14336=DIRECTION('ref_axis',(0.5,0.,-0.866025403784439));
#14337=DIRECTION('center_axis',(0.,1.,0.));
#14338=DIRECTION('ref_axis',(0.5,0.,-0.866025403784438));
#14339=DIRECTION('center_axis',(0.,1.,0.));
#14340=DIRECTION('ref_axis',(0.5,0.,-0.866025403784439));
#14341=DIRECTION('center_axis',(0.,1.,0.));
#14342=DIRECTION('ref_axis',(0.5,0.,-0.866025403784438));
#14343=DIRECTION('center_axis',(0.,1.,0.));
#14344=DIRECTION('ref_axis',(0.5,0.,-0.866025403784439));
#14345=DIRECTION('center_axis',(0.,1.,0.));
#14346=DIRECTION('ref_axis',(0.5,0.,-0.866025403784438));
#14347=DIRECTION('center_axis',(0.,1.,0.));
#14348=DIRECTION('ref_axis',(0.5,0.,-0.866025403784439));
#14349=DIRECTION('center_axis',(0.,1.,0.));
#14350=DIRECTION('ref_axis',(0.5,0.,-0.866025403784438));
#14351=DIRECTION('center_axis',(0.,1.,0.));
#14352=DIRECTION('ref_axis',(0.5,0.,-0.866025403784439));
#14353=DIRECTION('center_axis',(0.,1.,0.));
#14354=DIRECTION('ref_axis',(0.5,0.,-0.866025403784438));
#14355=DIRECTION('center_axis',(0.,1.,0.));
#14356=DIRECTION('ref_axis',(0.5,0.,-0.866025403784439));
#14357=DIRECTION('center_axis',(0.,1.,0.));
#14358=DIRECTION('ref_axis',(0.5,0.,-0.866025403784438));
#14359=DIRECTION('center_axis',(-0.762527203906389,0.,0.646956152534857));
#14360=DIRECTION('ref_axis',(0.646956152534857,0.,0.762527203906389));
#14361=DIRECTION('',(0.646956152534857,0.,0.762527203906389));
#14362=DIRECTION('',(0.,1.,0.));
#14363=DIRECTION('',(0.,1.,0.));
#14364=DIRECTION('center_axis',(-0.695442635009612,0.,0.718581617779698));
#14365=DIRECTION('ref_axis',(0.718581617779698,0.,0.695442635009612));
#14366=DIRECTION('',(0.718581617779698,0.,0.695442635009612));
#14367=DIRECTION('',(0.,1.,0.));
#14368=DIRECTION('center_axis',(-0.621660573370078,0.,0.78328674922865));
#14369=DIRECTION('ref_axis',(0.78328674922865,0.,0.621660573370078));
#14370=DIRECTION('',(0.78328674922865,0.,0.621660573370078));
#14371=DIRECTION('',(0.,1.,0.));
#14372=DIRECTION('center_axis',(-0.541891580574752,0.,0.840448401094438));
#14373=DIRECTION('ref_axis',(0.840448401094438,0.,0.541891580574752));
#14374=DIRECTION('',(0.840448401094438,0.,0.541891580574752));
#14375=DIRECTION('',(0.,1.,0.));
#14376=DIRECTION('center_axis',(-0.456903875630421,0.,0.889516075421856));
#14377=DIRECTION('ref_axis',(0.889516075421856,0.,0.456903875630421));
#14378=DIRECTION('',(0.889516075421856,0.,0.456903875630421));
#14379=DIRECTION('',(0.,1.,0.));
#14380=DIRECTION('center_axis',(-0.367515936594704,0.,0.930017223684012));
#14381=DIRECTION('ref_axis',(0.930017223684012,0.,0.367515936594704));
#14382=DIRECTION('',(0.930017223684012,0.,0.367515936594704));
#14383=DIRECTION('',(0.,1.,0.));
#14384=DIRECTION('center_axis',(-0.274588618184932,0.,0.961561797682962));
#14385=DIRECTION('ref_axis',(0.961561797682962,0.,0.274588618184932));
#14386=DIRECTION('',(0.961561797682962,0.,0.274588618184932));
#14387=DIRECTION('',(0.,1.,0.));
#14388=DIRECTION('center_axis',(-0.179016861276632,0.,0.983846005927078));
#14389=DIRECTION('ref_axis',(0.983846005927078,0.,0.179016861276632));
#14390=DIRECTION('',(0.983846005927077,0.,0.179016861276632));
#14391=DIRECTION('',(0.,1.,0.));
#14392=DIRECTION('center_axis',(-0.99144486137381,0.,-0.130526192220052));
#14393=DIRECTION('ref_axis',(-0.130526192220052,0.,0.99144486137381));
#14394=DIRECTION('',(-0.130526192220052,0.,0.99144486137381));
#14395=DIRECTION('',(0.,1.,0.));
#14396=DIRECTION('center_axis',(0.179016861276632,0.,-0.983846005927078));
#14397=DIRECTION('ref_axis',(-0.983846005927078,0.,-0.179016861276632));
#14398=DIRECTION('',(-0.983846005927078,0.,-0.179016861276632));
#14399=DIRECTION('',(-0.983846005927078,0.,-0.179016861276632));
#14400=DIRECTION('',(0.,1.,0.));
#14401=DIRECTION('center_axis',(0.274588618184932,0.,-0.961561797682962));
#14402=DIRECTION('ref_axis',(-0.961561797682962,0.,-0.274588618184932));
#14403=DIRECTION('',(-0.961561797682962,0.,-0.274588618184932));
#14404=DIRECTION('',(-0.961561797682962,0.,-0.274588618184932));
#14405=DIRECTION('',(0.,1.,0.));
#14406=DIRECTION('center_axis',(0.367515936594703,0.,-0.930017223684013));
#14407=DIRECTION('ref_axis',(-0.930017223684013,0.,-0.367515936594703));
#14408=DIRECTION('',(-0.930017223684013,0.,-0.367515936594703));
#14409=DIRECTION('',(-0.930017223684013,0.,-0.367515936594703));
#14410=DIRECTION('',(0.,1.,0.));
#14411=DIRECTION('center_axis',(0.456903875630423,0.,-0.889516075421855));
#14412=DIRECTION('ref_axis',(-0.889516075421855,0.,-0.456903875630423));
#14413=DIRECTION('',(-0.889516075421855,0.,-0.456903875630423));
#14414=DIRECTION('',(-0.889516075421855,0.,-0.456903875630423));
#14415=DIRECTION('',(0.,1.,0.));
#14416=DIRECTION('center_axis',(0.54189158057475,0.,-0.840448401094439));
#14417=DIRECTION('ref_axis',(-0.840448401094439,0.,-0.54189158057475));
#14418=DIRECTION('',(-0.840448401094439,0.,-0.54189158057475));
#14419=DIRECTION('',(-0.840448401094439,0.,-0.54189158057475));
#14420=DIRECTION('',(0.,1.,0.));
#14421=DIRECTION('center_axis',(0.621660573370078,0.,-0.78328674922865));
#14422=DIRECTION('ref_axis',(-0.78328674922865,0.,-0.621660573370078));
#14423=DIRECTION('',(-0.78328674922865,0.,-0.621660573370078));
#14424=DIRECTION('',(-0.78328674922865,0.,-0.621660573370078));
#14425=DIRECTION('',(0.,1.,0.));
#14426=DIRECTION('center_axis',(0.695442635009612,0.,-0.718581617779698));
#14427=DIRECTION('ref_axis',(-0.718581617779698,0.,-0.695442635009612));
#14428=DIRECTION('',(-0.718581617779698,0.,-0.695442635009612));
#14429=DIRECTION('',(-0.718581617779698,0.,-0.695442635009612));
#14430=DIRECTION('',(0.,1.,0.));
#14431=DIRECTION('center_axis',(0.762527203906389,0.,-0.646956152534857));
#14432=DIRECTION('ref_axis',(-0.646956152534857,0.,-0.762527203906389));
#14433=DIRECTION('',(-0.646956152534857,0.,-0.762527203906389));
#14434=DIRECTION('',(-0.646956152534857,0.,-0.762527203906389));
#14435=DIRECTION('',(0.,1.,0.));
#14436=DIRECTION('center_axis',(0.60876142900872,0.,0.793353340291235));
#14437=DIRECTION('ref_axis',(0.793353340291235,0.,-0.60876142900872));
#14438=DIRECTION('',(0.793353340291235,0.,-0.60876142900872));
#14439=DIRECTION('center_axis',(0.,1.,0.));
#14440=DIRECTION('ref_axis',(0.5,0.,-0.866025403784439));
#14441=DIRECTION('center_axis',(0.,1.,0.));
#14442=DIRECTION('ref_axis',(0.5,0.,-0.866025403784439));
#14443=DIRECTION('center_axis',(0.,1.,0.));
#14444=DIRECTION('ref_axis',(0.5,0.,-0.866025403784438));
#14445=DIRECTION('center_axis',(0.,1.,0.));
#14446=DIRECTION('ref_axis',(0.5,0.,-0.866025403784439));
#14447=DIRECTION('center_axis',(0.,1.,0.));
#14448=DIRECTION('ref_axis',(0.5,0.,-0.866025403784438));
#14449=DIRECTION('center_axis',(0.,1.,0.));
#14450=DIRECTION('ref_axis',(0.5,0.,-0.866025403784439));
#14451=DIRECTION('center_axis',(0.,1.,0.));
#14452=DIRECTION('ref_axis',(0.5,0.,-0.866025403784438));
#14453=DIRECTION('center_axis',(0.,1.,0.));
#14454=DIRECTION('ref_axis',(0.5,0.,-0.866025403784439));
#14455=DIRECTION('center_axis',(0.,1.,0.));
#14456=DIRECTION('ref_axis',(0.5,0.,-0.866025403784438));
#14457=DIRECTION('center_axis',(0.,1.,0.));
#14458=DIRECTION('ref_axis',(0.5,0.,-0.866025403784439));
#14459=DIRECTION('center_axis',(0.,1.,0.));
#14460=DIRECTION('ref_axis',(0.5,0.,-0.866025403784438));
#14461=DIRECTION('center_axis',(0.,1.,0.));
#14462=DIRECTION('ref_axis',(0.5,0.,-0.866025403784439));
#14463=DIRECTION('center_axis',(0.,1.,0.));
#14464=DIRECTION('ref_axis',(0.5,0.,-0.866025403784438));
#14465=DIRECTION('center_axis',(0.,1.,0.));
#14466=DIRECTION('ref_axis',(0.5,0.,-0.866025403784439));
#14467=DIRECTION('center_axis',(0.,1.,0.));
#14468=DIRECTION('ref_axis',(0.5,0.,-0.866025403784438));
#14469=DIRECTION('center_axis',(0.,1.,0.));
#14470=DIRECTION('ref_axis',(0.5,0.,-0.866025403784439));
#14471=DIRECTION('center_axis',(0.,1.,0.));
#14472=DIRECTION('ref_axis',(0.5,0.,-0.866025403784438));
#14473=DIRECTION('center_axis',(0.,1.,0.));
#14474=DIRECTION('ref_axis',(0.5,0.,-0.866025403784438));
#14475=DIRECTION('center_axis',(0.,1.,0.));
#14476=DIRECTION('ref_axis',(0.5,0.,-0.866025403784438));
#14477=DIRECTION('',(0.,-1.,0.));
#14478=DIRECTION('center_axis',(0.,1.,0.));
#14479=DIRECTION('ref_axis',(0.5,0.,-0.866025403784439));
#14480=DIRECTION('axis',(0.,0.,1.));
#14481=DIRECTION('refdir',(1.,0.,0.));
#14482=DIRECTION('center_axis',(0.,1.,0.));
#14483=DIRECTION('ref_axis',(0.866025403784439,0.,-0.5));
#14484=DIRECTION('',(0.121869343405147,0.,0.992546151641322));
#14485=DIRECTION('',(0.994821748296033,0.,-0.101635078182804));
#14486=DIRECTION('',(0.998134798421867,0.,-0.0610485395348574));
#14487=DIRECTION('',(0.999792698085389,0.,-0.0203607675478923));
#14488=DIRECTION('',(0.999792698085388,0.,0.0203607675478936));
#14489=DIRECTION('',(0.998134798421867,0.,0.0610485395348586));
#14490=DIRECTION('',(0.994821748296033,0.,0.101635078182805));
#14491=DIRECTION('',(0.121869343405148,0.,-0.992546151641322));
#14492=DIRECTION('center_axis',(0.,-1.,0.));
#14493=DIRECTION('ref_axis',(0.866025403784439,0.,-0.5));
#14494=DIRECTION('',(-0.798635510047293,0.,0.601815023152048));
#14495=DIRECTION('',(0.585429433769943,0.,0.810723367170211));
#14496=DIRECTION('',(0.551936985312059,0.,0.833885822067168));
#14497=DIRECTION('',(0.517529290979719,0.,0.855665491286186));
#14498=DIRECTION('',(0.482263407105669,0.,0.876026258834079));
#14499=DIRECTION('',(0.446197813109808,0.,0.894934361602026));
#14500=DIRECTION('',(0.40939231452609,0.,0.912358445353015));
#14501=DIRECTION('',(0.92050485345244,0.,-0.390731128489274));
#14502=DIRECTION('center_axis',(0.,-1.,0.));
#14503=DIRECTION('ref_axis',(0.866025403784439,0.,-0.5));
#14504=DIRECTION('',(-0.92050485345244,0.,-0.390731128489274));
#14505=DIRECTION('',(-0.40939231452609,0.,0.912358445353015));
#14506=DIRECTION('',(-0.446197813109808,0.,0.894934361602025));
#14507=DIRECTION('',(-0.482263407105669,0.,0.876026258834078));
#14508=DIRECTION('',(-0.51752929097972,0.,0.855665491286185));
#14509=DIRECTION('',(-0.551936985312059,0.,0.833885822067168));
#14510=DIRECTION('',(-0.585429433769943,0.,0.810723367170211));
#14511=DIRECTION('',(0.798635510047293,0.,0.601815023152048));
#14512=DIRECTION('center_axis',(0.,-1.,0.));
#14513=DIRECTION('ref_axis',(0.866025403784439,0.,-0.5));
#14514=DIRECTION('',(-0.121869343405147,0.,-0.992546151641322));
#14515=DIRECTION('',(-0.994821748296033,0.,0.101635078182804));
#14516=DIRECTION('',(-0.998134798421867,0.,0.0610485395348577));
#14517=DIRECTION('',(-0.999792698085388,0.,0.0203607675478927));
#14518=DIRECTION('',(-0.999792698085389,0.,-0.0203607675478932));
#14519=DIRECTION('',(-0.998134798421867,0.,-0.0610485395348582));
#14520=DIRECTION('',(-0.994821748296033,0.,-0.101635078182805));
#14521=DIRECTION('',(-0.121869343405148,0.,0.992546151641322));
#14522=DIRECTION('center_axis',(0.,-1.,0.));
#14523=DIRECTION('ref_axis',(0.866025403784439,0.,-0.5));
#14524=DIRECTION('',(0.798635510047293,0.,-0.601815023152048));
#14525=DIRECTION('',(-0.585429433769943,0.,-0.810723367170211));
#14526=DIRECTION('',(-0.551936985312059,0.,-0.833885822067168));
#14527=DIRECTION('',(-0.517529290979719,0.,-0.855665491286186));
#14528=DIRECTION('',(-0.482263407105669,0.,-0.876026258834078));
#14529=DIRECTION('',(-0.446197813109808,0.,-0.894934361602026));
#14530=DIRECTION('',(-0.40939231452609,0.,-0.912358445353015));
#14531=DIRECTION('',(-0.92050485345244,0.,0.390731128489274));
#14532=DIRECTION('center_axis',(0.,-1.,0.));
#14533=DIRECTION('ref_axis',(0.866025403784439,0.,-0.5));
#14534=DIRECTION('',(0.92050485345244,0.,0.390731128489275));
#14535=DIRECTION('',(0.409392314526091,0.,-0.912358445353015));
#14536=DIRECTION('',(0.446197813109809,0.,-0.894934361602025));
#14537=DIRECTION('',(0.48226340710567,0.,-0.876026258834078));
#14538=DIRECTION('',(0.51752929097972,0.,-0.855665491286185));
#14539=DIRECTION('',(0.55193698531206,0.,-0.833885822067167));
#14540=DIRECTION('',(0.585429433769943,0.,-0.81072336717021));
#14541=DIRECTION('',(-0.798635510047292,0.,-0.601815023152049));
#14542=DIRECTION('center_axis',(0.,-1.,0.));
#14543=DIRECTION('ref_axis',(0.866025403784439,0.,-0.5));
#14544=DIRECTION('center_axis',(0.,1.,0.));
#14545=DIRECTION('ref_axis',(0.866025403784439,0.,-0.5));
#14546=DIRECTION('',(0.,-1.,0.));
#14547=DIRECTION('center_axis',(0.,1.,0.));
#14548=DIRECTION('ref_axis',(0.866025403784439,0.,-0.5));
#14549=DIRECTION('',(0.,1.,0.));
#14550=DIRECTION('center_axis',(0.,1.,0.));
#14551=DIRECTION('ref_axis',(0.866025403784439,0.,-0.5));
#14552=DIRECTION('',(0.,-1.,0.));
#14553=DIRECTION('center_axis',(0.,1.,0.));
#14554=DIRECTION('ref_axis',(0.866025403784439,0.,-0.5));
#14555=DIRECTION('',(0.,1.,0.));
#14556=DIRECTION('center_axis',(0.,1.,0.));
#14557=DIRECTION('ref_axis',(0.866025403784439,0.,-0.5));
#14558=DIRECTION('',(0.,-1.,0.));
#14559=DIRECTION('center_axis',(0.,1.,0.));
#14560=DIRECTION('ref_axis',(0.866025403784439,0.,-0.5));
#14561=DIRECTION('',(0.,1.,0.));
#14562=DIRECTION('center_axis',(0.,1.,0.));
#14563=DIRECTION('ref_axis',(0.866025403784439,0.,-0.5));
#14564=DIRECTION('',(0.,1.,0.));
#14565=DIRECTION('',(0.,-1.,0.));
#14566=DIRECTION('center_axis',(0.,1.,0.));
#14567=DIRECTION('ref_axis',(0.866025403784439,0.,-0.5));
#14568=DIRECTION('center_axis',(0.,1.,0.));
#14569=DIRECTION('ref_axis',(0.866025403784439,0.,-0.5));
#14570=DIRECTION('',(0.,1.,0.));
#14571=DIRECTION('',(0.,-1.,0.));
#14572=DIRECTION('center_axis',(0.,1.,0.));
#14573=DIRECTION('ref_axis',(0.866025403784439,0.,-0.5));
#14574=DIRECTION('center_axis',(0.,1.,0.));
#14575=DIRECTION('ref_axis',(0.866025403784439,0.,-0.5));
#14576=DIRECTION('',(0.,1.,0.));
#14577=DIRECTION('',(0.,-1.,0.));
#14578=DIRECTION('center_axis',(0.,1.,0.));
#14579=DIRECTION('ref_axis',(0.866025403784439,0.,-0.5));
#14580=DIRECTION('center_axis',(0.,1.,0.));
#14581=DIRECTION('ref_axis',(0.866025403784439,0.,-0.5));
#14582=DIRECTION('',(-0.121869343405147,0.,-0.992546151641322));
#14583=DIRECTION('',(0.798635510047292,0.,0.601815023152049));
#14584=DIRECTION('',(-0.585429433769943,0.,0.81072336717021));
#14585=DIRECTION('',(-0.55193698531206,0.,0.833885822067167));
#14586=DIRECTION('',(-0.51752929097972,0.,0.855665491286185));
#14587=DIRECTION('',(-0.48226340710567,0.,0.876026258834078));
#14588=DIRECTION('',(-0.446197813109809,0.,0.894934361602025));
#14589=DIRECTION('',(-0.409392314526091,0.,0.912358445353015));
#14590=DIRECTION('',(-0.92050485345244,0.,-0.390731128489275));
#14591=DIRECTION('',(0.92050485345244,0.,-0.390731128489274));
#14592=DIRECTION('',(0.40939231452609,0.,0.912358445353015));
#14593=DIRECTION('',(0.446197813109808,0.,0.894934361602026));
#14594=DIRECTION('',(0.482263407105669,0.,0.876026258834078));
#14595=DIRECTION('',(0.517529290979719,0.,0.855665491286186));
#14596=DIRECTION('',(0.551936985312059,0.,0.833885822067168));
#14597=DIRECTION('',(0.585429433769943,0.,0.810723367170211));
#14598=DIRECTION('',(-0.798635510047293,0.,0.601815023152048));
#14599=DIRECTION('',(0.121869343405148,0.,-0.992546151641322));
#14600=DIRECTION('',(0.994821748296033,0.,0.101635078182805));
#14601=DIRECTION('',(0.998134798421867,0.,0.0610485395348582));
#14602=DIRECTION('',(0.999792698085389,0.,0.0203607675478932));
#14603=DIRECTION('',(0.999792698085388,0.,-0.0203607675478927));
#14604=DIRECTION('',(0.998134798421867,0.,-0.0610485395348577));
#14605=DIRECTION('',(0.994821748296033,0.,-0.101635078182804));
#14606=DIRECTION('',(0.121869343405147,0.,0.992546151641322));
#14607=DIRECTION('',(-0.798635510047293,0.,-0.601815023152048));
#14608=DIRECTION('',(0.585429433769943,0.,-0.810723367170211));
#14609=DIRECTION('',(0.551936985312059,0.,-0.833885822067168));
#14610=DIRECTION('',(0.51752929097972,0.,-0.855665491286185));
#14611=DIRECTION('',(0.482263407105669,0.,-0.876026258834078));
#14612=DIRECTION('',(0.446197813109808,0.,-0.894934361602025));
#14613=DIRECTION('',(0.40939231452609,0.,-0.912358445353015));
#14614=DIRECTION('',(0.92050485345244,0.,0.390731128489274));
#14615=DIRECTION('',(-0.92050485345244,0.,0.390731128489274));
#14616=DIRECTION('',(-0.40939231452609,0.,-0.912358445353015));
#14617=DIRECTION('',(-0.446197813109808,0.,-0.894934361602026));
#14618=DIRECTION('',(-0.482263407105669,0.,-0.876026258834079));
#14619=DIRECTION('',(-0.517529290979719,0.,-0.855665491286186));
#14620=DIRECTION('',(-0.551936985312059,0.,-0.833885822067168));
#14621=DIRECTION('',(-0.585429433769943,0.,-0.810723367170211));
#14622=DIRECTION('',(0.798635510047293,0.,-0.601815023152048));
#14623=DIRECTION('',(-0.121869343405148,0.,0.992546151641322));
#14624=DIRECTION('',(-0.994821748296033,0.,-0.101635078182805));
#14625=DIRECTION('',(-0.998134798421867,0.,-0.0610485395348586));
#14626=DIRECTION('',(-0.999792698085388,0.,-0.0203607675478936));
#14627=DIRECTION('',(-0.999792698085389,0.,0.0203607675478923));
#14628=DIRECTION('',(-0.998134798421867,0.,0.0610485395348574));
#14629=DIRECTION('',(-0.994821748296033,0.,0.101635078182804));
#14630=DIRECTION('center_axis',(0.390731128489275,0.,-0.92050485345244));
#14631=DIRECTION('ref_axis',(-0.92050485345244,0.,-0.390731128489275));
#14632=DIRECTION('',(0.,1.,0.));
#14633=DIRECTION('',(-0.92050485345244,0.,-0.390731128489275));
#14634=DIRECTION('',(0.,1.,0.));
#14635=DIRECTION('',(0.92050485345244,0.,0.390731128489275));
#14636=DIRECTION('',(0.,1.,0.));
#14637=DIRECTION('center_axis',(-0.912358445353015,0.,-0.409392314526091));
#14638=DIRECTION('ref_axis',(-0.409392314526091,0.,0.912358445353015));
#14639=DIRECTION('',(0.,1.,0.));
#14640=DIRECTION('',(-0.409392314526091,0.,0.912358445353015));
#14641=DIRECTION('center_axis',(-0.912358445353015,0.,-0.409392314526091));
#14642=DIRECTION('ref_axis',(-0.409392314526091,0.,0.912358445353015));
#14643=DIRECTION('',(0.409392314526091,0.,-0.912358445353015));
#14644=DIRECTION('',(0.,1.,0.));
#14645=DIRECTION('center_axis',(-0.894934361602025,0.,-0.446197813109809));
#14646=DIRECTION('ref_axis',(-0.446197813109809,0.,0.894934361602025));
#14647=DIRECTION('',(0.,1.,0.));
#14648=DIRECTION('',(-0.446197813109809,0.,0.894934361602025));
#14649=DIRECTION('center_axis',(-0.876026258834078,0.,-0.48226340710567));
#14650=DIRECTION('ref_axis',(-0.48226340710567,0.,0.876026258834078));
#14651=DIRECTION('',(0.,1.,0.));
#14652=DIRECTION('',(-0.48226340710567,0.,0.876026258834078));
#14653=DIRECTION('center_axis',(-0.855665491286185,0.,-0.51752929097972));
#14654=DIRECTION('ref_axis',(-0.51752929097972,0.,0.855665491286185));
#14655=DIRECTION('',(0.,1.,0.));
#14656=DIRECTION('',(-0.51752929097972,0.,0.855665491286185));
#14657=DIRECTION('center_axis',(-0.833885822067167,0.,-0.55193698531206));
#14658=DIRECTION('ref_axis',(-0.55193698531206,0.,0.833885822067167));
#14659=DIRECTION('',(0.,1.,0.));
#14660=DIRECTION('',(-0.55193698531206,0.,0.833885822067167));
#14661=DIRECTION('center_axis',(-0.81072336717021,0.,-0.585429433769943));
#14662=DIRECTION('ref_axis',(-0.585429433769943,0.,0.81072336717021));
#14663=DIRECTION('',(0.,-1.,0.));
#14664=DIRECTION('',(-0.585429433769944,0.,0.81072336717021));
#14665=DIRECTION('center_axis',(0.,-1.,0.));
#14666=DIRECTION('ref_axis',(0.500000000000001,0.,-0.866025403784438));
#14667=DIRECTION('',(-0.798635510047292,0.,-0.601815023152049));
#14668=DIRECTION('',(0.585429433769944,0.,-0.81072336717021));
#14669=DIRECTION('',(0.55193698531206,0.,-0.833885822067167));
#14670=DIRECTION('',(0.51752929097972,0.,-0.855665491286185));
#14671=DIRECTION('',(0.48226340710567,0.,-0.876026258834078));
#14672=DIRECTION('',(0.446197813109809,0.,-0.894934361602025));
#14673=DIRECTION('',(-0.409392314526095,0.,0.912358445353013));
#14674=DIRECTION('',(-0.446197813109808,0.,0.894934361602026));
#14675=DIRECTION('',(-0.48226340710567,0.,0.876026258834078));
#14676=DIRECTION('',(-0.51752929097972,0.,0.855665491286185));
#14677=DIRECTION('',(-0.551936985312061,0.,0.833885822067167));
#14678=DIRECTION('',(-0.58542943376994,0.,0.810723367170213));
#14679=DIRECTION('center_axis',(-0.81072336717021,0.,-0.585429433769943));
#14680=DIRECTION('ref_axis',(-0.585429433769943,0.,0.81072336717021));
#14681=DIRECTION('',(0.,1.,0.));
#14682=DIRECTION('',(0.,-1.,0.));
#14683=DIRECTION('center_axis',(-0.833885822067167,0.,-0.55193698531206));
#14684=DIRECTION('ref_axis',(-0.55193698531206,0.,0.833885822067167));
#14685=DIRECTION('',(0.,1.,0.));
#14686=DIRECTION('center_axis',(-0.855665491286185,0.,-0.51752929097972));
#14687=DIRECTION('ref_axis',(-0.51752929097972,0.,0.855665491286185));
#14688=DIRECTION('',(0.,1.,0.));
#14689=DIRECTION('center_axis',(-0.876026258834078,0.,-0.48226340710567));
#14690=DIRECTION('ref_axis',(-0.48226340710567,0.,0.876026258834078));
#14691=DIRECTION('',(0.,1.,0.));
#14692=DIRECTION('center_axis',(-0.894934361602025,0.,-0.446197813109809));
#14693=DIRECTION('ref_axis',(-0.446197813109809,0.,0.894934361602025));
#14694=DIRECTION('center_axis',(0.912358445353013,0.,0.409392314526095));
#14695=DIRECTION('ref_axis',(0.409392314526095,0.,-0.912358445353013));
#14696=DIRECTION('',(0.409392314526095,0.,-0.912358445353013));
#14697=DIRECTION('',(0.,1.,0.));
#14698=DIRECTION('center_axis',(0.894934361602026,0.,0.446197813109808));
#14699=DIRECTION('ref_axis',(0.446197813109808,0.,-0.894934361602026));
#14700=DIRECTION('',(0.446197813109808,0.,-0.894934361602026));
#14701=DIRECTION('',(0.,1.,0.));
#14702=DIRECTION('center_axis',(0.876026258834078,0.,0.48226340710567));
#14703=DIRECTION('ref_axis',(0.48226340710567,0.,-0.876026258834078));
#14704=DIRECTION('',(0.48226340710567,0.,-0.876026258834078));
#14705=DIRECTION('',(0.,1.,0.));
#14706=DIRECTION('center_axis',(0.855665491286185,0.,0.51752929097972));
#14707=DIRECTION('ref_axis',(0.51752929097972,0.,-0.855665491286185));
#14708=DIRECTION('',(0.51752929097972,0.,-0.855665491286185));
#14709=DIRECTION('',(0.,1.,0.));
#14710=DIRECTION('center_axis',(0.833885822067167,0.,0.551936985312061));
#14711=DIRECTION('ref_axis',(0.551936985312061,0.,-0.833885822067167));
#14712=DIRECTION('',(0.551936985312061,0.,-0.833885822067167));
#14713=DIRECTION('',(0.,1.,0.));
#14714=DIRECTION('center_axis',(0.810723367170213,0.,0.58542943376994));
#14715=DIRECTION('ref_axis',(0.58542943376994,0.,-0.810723367170213));
#14716=DIRECTION('',(0.58542943376994,0.,-0.810723367170213));
#14717=DIRECTION('',(0.,1.,0.));
#14718=DIRECTION('center_axis',(-0.601815023152049,0.,0.798635510047292));
#14719=DIRECTION('ref_axis',(0.798635510047292,0.,0.601815023152049));
#14720=DIRECTION('',(0.798635510047292,0.,0.601815023152049));
#14721=DIRECTION('center_axis',(0.,1.,0.));
#14722=DIRECTION('ref_axis',(-0.500000000000001,0.,0.866025403784438));
#14723=DIRECTION('center_axis',(0.601815023152048,0.,0.798635510047293));
#14724=DIRECTION('ref_axis',(0.798635510047293,0.,-0.601815023152048));
#14725=DIRECTION('',(0.,1.,0.));
#14726=DIRECTION('',(0.798635510047293,0.,-0.601815023152048));
#14727=DIRECTION('',(0.,1.,0.));
#14728=DIRECTION('',(-0.798635510047293,0.,0.601815023152048));
#14729=DIRECTION('',(0.,1.,0.));
#14730=DIRECTION('center_axis',(0.810723367170211,0.,-0.585429433769943));
#14731=DIRECTION('ref_axis',(-0.585429433769943,0.,-0.810723367170211));
#14732=DIRECTION('',(0.,1.,0.));
#14733=DIRECTION('',(-0.585429433769943,0.,-0.810723367170211));
#14734=DIRECTION('center_axis',(0.810723367170211,0.,-0.585429433769943));
#14735=DIRECTION('ref_axis',(-0.585429433769943,0.,-0.810723367170211));
#14736=DIRECTION('',(0.585429433769943,0.,0.810723367170211));
#14737=DIRECTION('',(0.,1.,0.));
#14738=DIRECTION('center_axis',(0.833885822067168,0.,-0.551936985312059));
#14739=DIRECTION('ref_axis',(-0.551936985312059,0.,-0.833885822067168));
#14740=DIRECTION('',(0.,1.,0.));
#14741=DIRECTION('',(-0.551936985312059,0.,-0.833885822067168));
#14742=DIRECTION('center_axis',(0.855665491286186,0.,-0.517529290979719));
#14743=DIRECTION('ref_axis',(-0.517529290979719,0.,-0.855665491286186));
#14744=DIRECTION('',(0.,1.,0.));
#14745=DIRECTION('',(-0.517529290979719,0.,-0.855665491286186));
#14746=DIRECTION('center_axis',(0.876026258834078,0.,-0.482263407105669));
#14747=DIRECTION('ref_axis',(-0.482263407105669,0.,-0.876026258834079));
#14748=DIRECTION('',(0.,1.,0.));
#14749=DIRECTION('',(-0.482263407105669,0.,-0.876026258834079));
#14750=DIRECTION('center_axis',(0.894934361602026,0.,-0.446197813109808));
#14751=DIRECTION('ref_axis',(-0.446197813109808,0.,-0.894934361602026));
#14752=DIRECTION('',(0.,1.,0.));
#14753=DIRECTION('',(-0.446197813109808,0.,-0.894934361602026));
#14754=DIRECTION('center_axis',(0.912358445353015,0.,-0.40939231452609));
#14755=DIRECTION('ref_axis',(-0.40939231452609,0.,-0.912358445353015));
#14756=DIRECTION('',(0.,-1.,0.));
#14757=DIRECTION('',(-0.40939231452609,0.,-0.912358445353015));
#14758=DIRECTION('center_axis',(0.,-1.,0.));
#14759=DIRECTION('ref_axis',(0.5,0.,0.866025403784439));
#14760=DIRECTION('',(0.92050485345244,0.,-0.390731128489274));
#14761=DIRECTION('',(0.40939231452609,0.,0.912358445353015));
#14762=DIRECTION('',(0.446197813109808,0.,0.894934361602026));
#14763=DIRECTION('',(0.482263407105669,0.,0.876026258834079));
#14764=DIRECTION('',(0.517529290979719,0.,0.855665491286186));
#14765=DIRECTION('',(0.551936985312059,0.,0.833885822067168));
#14766=DIRECTION('',(-0.585429433769939,0.,-0.810723367170213));
#14767=DIRECTION('',(-0.55193698531206,0.,-0.833885822067167));
#14768=DIRECTION('',(-0.517529290979719,0.,-0.855665491286186));
#14769=DIRECTION('',(-0.482263407105669,0.,-0.876026258834078));
#14770=DIRECTION('',(-0.446197813109807,0.,-0.894934361602026));
#14771=DIRECTION('',(-0.409392314526094,0.,-0.912358445353014));
#14772=DIRECTION('center_axis',(0.912358445353015,0.,-0.40939231452609));
#14773=DIRECTION('ref_axis',(-0.40939231452609,0.,-0.912358445353015));
#14774=DIRECTION('',(0.,1.,0.));
#14775=DIRECTION('',(0.,-1.,0.));
#14776=DIRECTION('center_axis',(0.894934361602026,0.,-0.446197813109808));
#14777=DIRECTION('ref_axis',(-0.446197813109808,0.,-0.894934361602026));
#14778=DIRECTION('',(0.,1.,0.));
#14779=DIRECTION('center_axis',(0.876026258834078,0.,-0.482263407105669));
#14780=DIRECTION('ref_axis',(-0.482263407105669,0.,-0.876026258834079));
#14781=DIRECTION('',(0.,1.,0.));
#14782=DIRECTION('center_axis',(0.855665491286186,0.,-0.517529290979719));
#14783=DIRECTION('ref_axis',(-0.517529290979719,0.,-0.855665491286186));
#14784=DIRECTION('',(0.,1.,0.));
#14785=DIRECTION('center_axis',(0.833885822067168,0.,-0.551936985312059));
#14786=DIRECTION('ref_axis',(-0.551936985312059,0.,-0.833885822067168));
#14787=DIRECTION('center_axis',(-0.810723367170213,0.,0.585429433769939));
#14788=DIRECTION('ref_axis',(0.585429433769939,0.,0.810723367170213));
#14789=DIRECTION('',(0.585429433769939,0.,0.810723367170213));
#14790=DIRECTION('',(0.,1.,0.));
#14791=DIRECTION('center_axis',(-0.833885822067167,0.,0.55193698531206));
#14792=DIRECTION('ref_axis',(0.55193698531206,0.,0.833885822067167));
#14793=DIRECTION('',(0.55193698531206,0.,0.833885822067167));
#14794=DIRECTION('',(0.,1.,0.));
#14795=DIRECTION('center_axis',(-0.855665491286186,0.,0.517529290979719));
#14796=DIRECTION('ref_axis',(0.517529290979719,0.,0.855665491286186));
#14797=DIRECTION('',(0.517529290979719,0.,0.855665491286186));
#14798=DIRECTION('',(0.,1.,0.));
#14799=DIRECTION('center_axis',(-0.876026258834078,0.,0.482263407105669));
#14800=DIRECTION('ref_axis',(0.482263407105669,0.,0.876026258834078));
#14801=DIRECTION('',(0.482263407105669,0.,0.876026258834078));
#14802=DIRECTION('',(0.,1.,0.));
#14803=DIRECTION('center_axis',(-0.894934361602026,0.,0.446197813109807));
#14804=DIRECTION('ref_axis',(0.446197813109807,0.,0.894934361602026));
#14805=DIRECTION('',(0.446197813109807,0.,0.894934361602026));
#14806=DIRECTION('',(0.,1.,0.));
#14807=DIRECTION('center_axis',(-0.912358445353014,0.,0.409392314526094));
#14808=DIRECTION('ref_axis',(0.409392314526094,0.,0.912358445353014));
#14809=DIRECTION('',(0.409392314526094,0.,0.912358445353014));
#14810=DIRECTION('',(0.,1.,0.));
#14811=DIRECTION('center_axis',(-0.390731128489274,0.,-0.92050485345244));
#14812=DIRECTION('ref_axis',(-0.92050485345244,0.,0.390731128489274));
#14813=DIRECTION('',(-0.92050485345244,0.,0.390731128489274));
#14814=DIRECTION('center_axis',(0.,1.,0.));
#14815=DIRECTION('ref_axis',(-0.5,0.,-0.866025403784439));
#14816=DIRECTION('center_axis',(-0.992546151641322,0.,0.121869343405147));
#14817=DIRECTION('ref_axis',(0.121869343405147,0.,0.992546151641322));
#14818=DIRECTION('',(0.,1.,0.));
#14819=DIRECTION('',(0.121869343405147,0.,0.992546151641322));
#14820=DIRECTION('',(0.,1.,0.));
#14821=DIRECTION('',(-0.121869343405147,0.,-0.992546151641322));
#14822=DIRECTION('',(0.,1.,0.));
#14823=DIRECTION('center_axis',(0.101635078182804,0.,0.994821748296033));
#14824=DIRECTION('ref_axis',(0.994821748296033,0.,-0.101635078182804));
#14825=DIRECTION('',(0.,1.,0.));
#14826=DIRECTION('',(0.994821748296033,0.,-0.101635078182804));
#14827=DIRECTION('center_axis',(0.101635078182804,0.,0.994821748296033));
#14828=DIRECTION('ref_axis',(0.994821748296033,0.,-0.101635078182804));
#14829=DIRECTION('',(-0.994821748296033,0.,0.101635078182804));
#14830=DIRECTION('',(0.,1.,0.));
#14831=DIRECTION('center_axis',(0.0610485395348577,0.,0.998134798421867));
#14832=DIRECTION('ref_axis',(0.998134798421867,0.,-0.0610485395348577));
#14833=DIRECTION('',(0.,1.,0.));
#14834=DIRECTION('',(0.998134798421867,0.,-0.0610485395348577));
#14835=DIRECTION('center_axis',(0.0203607675478927,0.,0.999792698085389));
#14836=DIRECTION('ref_axis',(0.999792698085388,0.,-0.0203607675478927));
#14837=DIRECTION('',(0.,1.,0.));
#14838=DIRECTION('',(0.999792698085388,0.,-0.0203607675478927));
#14839=DIRECTION('center_axis',(-0.0203607675478932,0.,0.999792698085389));
#14840=DIRECTION('ref_axis',(0.999792698085389,0.,0.0203607675478932));
#14841=DIRECTION('',(0.,1.,0.));
#14842=DIRECTION('',(0.999792698085389,0.,0.0203607675478932));
#14843=DIRECTION('center_axis',(-0.0610485395348582,0.,0.998134798421867));
#14844=DIRECTION('ref_axis',(0.998134798421867,0.,0.0610485395348582));
#14845=DIRECTION('',(0.,1.,0.));
#14846=DIRECTION('',(0.998134798421867,0.,0.0610485395348582));
#14847=DIRECTION('center_axis',(-0.101635078182805,0.,0.994821748296033));
#14848=DIRECTION('ref_axis',(0.994821748296033,0.,0.101635078182805));
#14849=DIRECTION('',(0.,-1.,0.));
#14850=DIRECTION('',(0.994821748296033,0.,0.101635078182805));
#14851=DIRECTION('center_axis',(0.,-1.,0.));
#14852=DIRECTION('ref_axis',(-1.,0.,-2.22044604925031E-16));
#14853=DIRECTION('',(-0.121869343405148,0.,0.992546151641322));
#14854=DIRECTION('',(-0.994821748296033,0.,-0.101635078182805));
#14855=DIRECTION('',(-0.998134798421867,0.,-0.0610485395348582));
#14856=DIRECTION('',(-0.999792698085389,0.,-0.0203607675478932));
#14857=DIRECTION('',(-0.999792698085388,0.,0.0203607675478927));
#14858=DIRECTION('',(-0.998134798421867,0.,0.0610485395348577));
#14859=DIRECTION('',(0.994821748296033,0.,-0.1016350781828));
#14860=DIRECTION('',(0.998134798421867,0.,-0.0610485395348589));
#14861=DIRECTION('',(0.999792698085388,0.,-0.0203607675478925));
#14862=DIRECTION('',(0.999792698085389,0.,0.0203607675478929));
#14863=DIRECTION('',(0.998134798421867,0.,0.0610485395348593));
#14864=DIRECTION('',(0.994821748296033,0.,0.1016350781828));
#14865=DIRECTION('center_axis',(-0.101635078182805,0.,0.994821748296033));
#14866=DIRECTION('ref_axis',(0.994821748296033,0.,0.101635078182805));
#14867=DIRECTION('',(0.,1.,0.));
#14868=DIRECTION('',(0.,-1.,0.));
#14869=DIRECTION('center_axis',(-0.0610485395348582,0.,0.998134798421867));
#14870=DIRECTION('ref_axis',(0.998134798421867,0.,0.0610485395348582));
#14871=DIRECTION('',(0.,1.,0.));
#14872=DIRECTION('center_axis',(-0.0203607675478932,0.,0.999792698085389));
#14873=DIRECTION('ref_axis',(0.999792698085389,0.,0.0203607675478932));
#14874=DIRECTION('',(0.,1.,0.));
#14875=DIRECTION('center_axis',(0.0203607675478927,0.,0.999792698085389));
#14876=DIRECTION('ref_axis',(0.999792698085388,0.,-0.0203607675478927));
#14877=DIRECTION('',(0.,1.,0.));
#14878=DIRECTION('center_axis',(0.0610485395348577,0.,0.998134798421867));
#14879=DIRECTION('ref_axis',(0.998134798421867,0.,-0.0610485395348577));
#14880=DIRECTION('center_axis',(-0.1016350781828,0.,-0.994821748296033));
#14881=DIRECTION('ref_axis',(-0.994821748296033,0.,0.1016350781828));
#14882=DIRECTION('',(-0.994821748296033,0.,0.1016350781828));
#14883=DIRECTION('',(0.,1.,0.));
#14884=DIRECTION('center_axis',(-0.0610485395348589,0.,-0.998134798421867));
#14885=DIRECTION('ref_axis',(-0.998134798421867,0.,0.0610485395348589));
#14886=DIRECTION('',(-0.998134798421867,0.,0.0610485395348589));
#14887=DIRECTION('',(0.,1.,0.));
#14888=DIRECTION('center_axis',(-0.0203607675478925,0.,-0.999792698085389));
#14889=DIRECTION('ref_axis',(-0.999792698085388,0.,0.0203607675478925));
#14890=DIRECTION('',(-0.999792698085388,0.,0.0203607675478925));
#14891=DIRECTION('',(0.,1.,0.));
#14892=DIRECTION('center_axis',(0.0203607675478929,0.,-0.999792698085389));
#14893=DIRECTION('ref_axis',(-0.999792698085389,0.,-0.0203607675478929));
#14894=DIRECTION('',(-0.999792698085389,0.,-0.0203607675478929));
#14895=DIRECTION('',(0.,1.,0.));
#14896=DIRECTION('center_axis',(0.0610485395348593,0.,-0.998134798421867));
#14897=DIRECTION('ref_axis',(-0.998134798421867,0.,-0.0610485395348593));
#14898=DIRECTION('',(-0.998134798421867,0.,-0.0610485395348593));
#14899=DIRECTION('',(0.,1.,0.));
#14900=DIRECTION('center_axis',(0.1016350781828,0.,-0.994821748296033));
#14901=DIRECTION('ref_axis',(-0.994821748296033,0.,-0.1016350781828));
#14902=DIRECTION('',(-0.994821748296033,0.,-0.1016350781828));
#14903=DIRECTION('',(0.,1.,0.));
#14904=DIRECTION('center_axis',(0.992546151641322,0.,0.121869343405148));
#14905=DIRECTION('ref_axis',(0.121869343405148,0.,-0.992546151641322));
#14906=DIRECTION('',(0.121869343405148,0.,-0.992546151641322));
#14907=DIRECTION('center_axis',(0.,1.,0.));
#14908=DIRECTION('ref_axis',(1.,0.,2.22044604925031E-16));
#14909=DIRECTION('center_axis',(-0.601815023152048,0.,-0.798635510047293));
#14910=DIRECTION('ref_axis',(-0.798635510047293,0.,0.601815023152048));
#14911=DIRECTION('',(0.,1.,0.));
#14912=DIRECTION('',(-0.798635510047293,0.,0.601815023152048));
#14913=DIRECTION('',(0.,1.,0.));
#14914=DIRECTION('',(0.798635510047293,0.,-0.601815023152048));
#14915=DIRECTION('',(0.,1.,0.));
#14916=DIRECTION('center_axis',(-0.810723367170211,0.,0.585429433769943));
#14917=DIRECTION('ref_axis',(0.585429433769943,0.,0.810723367170211));
#14918=DIRECTION('',(0.,1.,0.));
#14919=DIRECTION('',(0.585429433769943,0.,0.810723367170211));
#14920=DIRECTION('center_axis',(-0.810723367170211,0.,0.585429433769943));
#14921=DIRECTION('ref_axis',(0.585429433769943,0.,0.810723367170211));
#14922=DIRECTION('',(-0.585429433769943,0.,-0.810723367170211));
#14923=DIRECTION('',(0.,1.,0.));
#14924=DIRECTION('center_axis',(-0.833885822067168,0.,0.551936985312059));
#14925=DIRECTION('ref_axis',(0.551936985312059,0.,0.833885822067168));
#14926=DIRECTION('',(0.,1.,0.));
#14927=DIRECTION('',(0.551936985312059,0.,0.833885822067168));
#14928=DIRECTION('center_axis',(-0.855665491286186,0.,0.517529290979719));
#14929=DIRECTION('ref_axis',(0.517529290979719,0.,0.855665491286186));
#14930=DIRECTION('',(0.,1.,0.));
#14931=DIRECTION('',(0.517529290979719,0.,0.855665491286186));
#14932=DIRECTION('center_axis',(-0.876026258834078,0.,0.482263407105669));
#14933=DIRECTION('ref_axis',(0.482263407105669,0.,0.876026258834078));
#14934=DIRECTION('',(0.,1.,0.));
#14935=DIRECTION('',(0.482263407105669,0.,0.876026258834078));
#14936=DIRECTION('center_axis',(-0.894934361602026,0.,0.446197813109808));
#14937=DIRECTION('ref_axis',(0.446197813109808,0.,0.894934361602026));
#14938=DIRECTION('',(0.,1.,0.));
#14939=DIRECTION('',(0.446197813109808,0.,0.894934361602026));
#14940=DIRECTION('center_axis',(-0.912358445353015,0.,0.40939231452609));
#14941=DIRECTION('ref_axis',(0.40939231452609,0.,0.912358445353015));
#14942=DIRECTION('',(0.,-1.,0.));
#14943=DIRECTION('',(0.40939231452609,0.,0.912358445353015));
#14944=DIRECTION('center_axis',(0.,-1.,0.));
#14945=DIRECTION('ref_axis',(-0.5,0.,-0.866025403784439));
#14946=DIRECTION('',(-0.92050485345244,0.,0.390731128489274));
#14947=DIRECTION('',(-0.40939231452609,0.,-0.912358445353015));
#14948=DIRECTION('',(-0.446197813109808,0.,-0.894934361602026));
#14949=DIRECTION('',(-0.482263407105669,0.,-0.876026258834078));
#14950=DIRECTION('',(-0.517529290979719,0.,-0.855665491286186));
#14951=DIRECTION('',(-0.551936985312059,0.,-0.833885822067168));
#14952=DIRECTION('',(0.585429433769939,0.,0.810723367170213));
#14953=DIRECTION('',(0.55193698531206,0.,0.833885822067167));
#14954=DIRECTION('',(0.517529290979719,0.,0.855665491286186));
#14955=DIRECTION('',(0.482263407105669,0.,0.876026258834078));
#14956=DIRECTION('',(0.446197813109807,0.,0.894934361602026));
#14957=DIRECTION('',(0.409392314526094,0.,0.912358445353014));
#14958=DIRECTION('center_axis',(-0.912358445353015,0.,0.40939231452609));
#14959=DIRECTION('ref_axis',(0.40939231452609,0.,0.912358445353015));
#14960=DIRECTION('',(0.,1.,0.));
#14961=DIRECTION('',(0.,-1.,0.));
#14962=DIRECTION('center_axis',(-0.894934361602026,0.,0.446197813109808));
#14963=DIRECTION('ref_axis',(0.446197813109808,0.,0.894934361602026));
#14964=DIRECTION('',(0.,1.,0.));
#14965=DIRECTION('center_axis',(-0.876026258834078,0.,0.482263407105669));
#14966=DIRECTION('ref_axis',(0.482263407105669,0.,0.876026258834078));
#14967=DIRECTION('',(0.,1.,0.));
#14968=DIRECTION('center_axis',(-0.855665491286186,0.,0.517529290979719));
#14969=DIRECTION('ref_axis',(0.517529290979719,0.,0.855665491286186));
#14970=DIRECTION('',(0.,1.,0.));
#14971=DIRECTION('center_axis',(-0.833885822067168,0.,0.551936985312059));
#14972=DIRECTION('ref_axis',(0.551936985312059,0.,0.833885822067168));
#14973=DIRECTION('center_axis',(0.810723367170213,0.,-0.585429433769939));
#14974=DIRECTION('ref_axis',(-0.585429433769939,0.,-0.810723367170213));
#14975=DIRECTION('',(-0.585429433769939,0.,-0.810723367170213));
#14976=DIRECTION('',(0.,1.,0.));
#14977=DIRECTION('center_axis',(0.833885822067167,0.,-0.55193698531206));
#14978=DIRECTION('ref_axis',(-0.55193698531206,0.,-0.833885822067167));
#14979=DIRECTION('',(-0.55193698531206,0.,-0.833885822067167));
#14980=DIRECTION('',(0.,1.,0.));
#14981=DIRECTION('center_axis',(0.855665491286186,0.,-0.517529290979719));
#14982=DIRECTION('ref_axis',(-0.517529290979719,0.,-0.855665491286186));
#14983=DIRECTION('',(-0.517529290979719,0.,-0.855665491286186));
#14984=DIRECTION('',(0.,1.,0.));
#14985=DIRECTION('center_axis',(0.876026258834078,0.,-0.482263407105669));
#14986=DIRECTION('ref_axis',(-0.482263407105669,0.,-0.876026258834078));
#14987=DIRECTION('',(-0.482263407105669,0.,-0.876026258834078));
#14988=DIRECTION('',(0.,1.,0.));
#14989=DIRECTION('center_axis',(0.894934361602026,0.,-0.446197813109807));
#14990=DIRECTION('ref_axis',(-0.446197813109807,0.,-0.894934361602026));
#14991=DIRECTION('',(-0.446197813109807,0.,-0.894934361602026));
#14992=DIRECTION('',(0.,1.,0.));
#14993=DIRECTION('center_axis',(0.912358445353014,0.,-0.409392314526094));
#14994=DIRECTION('ref_axis',(-0.409392314526094,0.,-0.912358445353014));
#14995=DIRECTION('',(-0.409392314526094,0.,-0.912358445353014));
#14996=DIRECTION('',(0.,1.,0.));
#14997=DIRECTION('center_axis',(0.390731128489274,0.,0.92050485345244));
#14998=DIRECTION('ref_axis',(0.92050485345244,0.,-0.390731128489274));
#14999=DIRECTION('',(0.92050485345244,0.,-0.390731128489274));
#15000=DIRECTION('center_axis',(0.,1.,0.));
#15001=DIRECTION('ref_axis',(0.5,0.,0.866025403784439));
#15002=DIRECTION('center_axis',(-0.390731128489274,0.,0.92050485345244));
#15003=DIRECTION('ref_axis',(0.92050485345244,0.,0.390731128489274));
#15004=DIRECTION('',(0.,1.,0.));
#15005=DIRECTION('',(0.92050485345244,0.,0.390731128489274));
#15006=DIRECTION('',(0.,1.,0.));
#15007=DIRECTION('',(-0.92050485345244,0.,-0.390731128489274));
#15008=DIRECTION('',(0.,1.,0.));
#15009=DIRECTION('center_axis',(0.912358445353015,0.,0.40939231452609));
#15010=DIRECTION('ref_axis',(0.40939231452609,0.,-0.912358445353015));
#15011=DIRECTION('',(0.,1.,0.));
#15012=DIRECTION('',(0.40939231452609,0.,-0.912358445353015));
#15013=DIRECTION('center_axis',(0.912358445353015,0.,0.40939231452609));
#15014=DIRECTION('ref_axis',(0.40939231452609,0.,-0.912358445353015));
#15015=DIRECTION('',(-0.40939231452609,0.,0.912358445353015));
#15016=DIRECTION('',(0.,1.,0.));
#15017=DIRECTION('center_axis',(0.894934361602025,0.,0.446197813109808));
#15018=DIRECTION('ref_axis',(0.446197813109808,0.,-0.894934361602025));
#15019=DIRECTION('',(0.,1.,0.));
#15020=DIRECTION('',(0.446197813109808,0.,-0.894934361602025));
#15021=DIRECTION('center_axis',(0.876026258834078,0.,0.482263407105669));
#15022=DIRECTION('ref_axis',(0.482263407105669,0.,-0.876026258834078));
#15023=DIRECTION('',(0.,1.,0.));
#15024=DIRECTION('',(0.482263407105669,0.,-0.876026258834078));
#15025=DIRECTION('center_axis',(0.855665491286185,0.,0.51752929097972));
#15026=DIRECTION('ref_axis',(0.51752929097972,0.,-0.855665491286185));
#15027=DIRECTION('',(0.,1.,0.));
#15028=DIRECTION('',(0.51752929097972,0.,-0.855665491286185));
#15029=DIRECTION('center_axis',(0.833885822067168,0.,0.551936985312059));
#15030=DIRECTION('ref_axis',(0.551936985312059,0.,-0.833885822067168));
#15031=DIRECTION('',(0.,1.,0.));
#15032=DIRECTION('',(0.551936985312059,0.,-0.833885822067167));
#15033=DIRECTION('center_axis',(0.810723367170211,0.,0.585429433769943));
#15034=DIRECTION('ref_axis',(0.585429433769943,0.,-0.810723367170211));
#15035=DIRECTION('',(0.,-1.,0.));
#15036=DIRECTION('',(0.585429433769943,0.,-0.810723367170211));
#15037=DIRECTION('center_axis',(0.,-1.,0.));
#15038=DIRECTION('ref_axis',(-0.5,0.,0.866025403784439));
#15039=DIRECTION('',(0.798635510047293,0.,0.601815023152048));
#15040=DIRECTION('',(-0.585429433769943,0.,0.810723367170211));
#15041=DIRECTION('',(-0.551936985312059,0.,0.833885822067167));
#15042=DIRECTION('',(-0.51752929097972,0.,0.855665491286185));
#15043=DIRECTION('',(-0.482263407105669,0.,0.876026258834078));
#15044=DIRECTION('',(-0.446197813109808,0.,0.894934361602025));
#15045=DIRECTION('',(0.409392314526094,0.,-0.912358445353013));
#15046=DIRECTION('',(0.446197813109807,0.,-0.894934361602026));
#15047=DIRECTION('',(0.48226340710567,0.,-0.876026258834078));
#15048=DIRECTION('',(0.517529290979719,0.,-0.855665491286185));
#15049=DIRECTION('',(0.55193698531206,0.,-0.833885822067167));
#15050=DIRECTION('',(0.58542943376994,0.,-0.810723367170213));
#15051=DIRECTION('center_axis',(0.810723367170211,0.,0.585429433769943));
#15052=DIRECTION('ref_axis',(0.585429433769943,0.,-0.810723367170211));
#15053=DIRECTION('',(0.,1.,0.));
#15054=DIRECTION('',(0.,-1.,0.));
#15055=DIRECTION('center_axis',(0.833885822067168,0.,0.551936985312059));
#15056=DIRECTION('ref_axis',(0.551936985312059,0.,-0.833885822067168));
#15057=DIRECTION('',(0.,1.,0.));
#15058=DIRECTION('center_axis',(0.855665491286185,0.,0.51752929097972));
#15059=DIRECTION('ref_axis',(0.51752929097972,0.,-0.855665491286185));
#15060=DIRECTION('',(0.,1.,0.));
#15061=DIRECTION('center_axis',(0.876026258834078,0.,0.482263407105669));
#15062=DIRECTION('ref_axis',(0.482263407105669,0.,-0.876026258834078));
#15063=DIRECTION('',(0.,1.,0.));
#15064=DIRECTION('center_axis',(0.894934361602025,0.,0.446197813109808));
#15065=DIRECTION('ref_axis',(0.446197813109808,0.,-0.894934361602025));
#15066=DIRECTION('center_axis',(-0.912358445353013,0.,-0.409392314526094));
#15067=DIRECTION('ref_axis',(-0.409392314526094,0.,0.912358445353013));
#15068=DIRECTION('',(-0.409392314526094,0.,0.912358445353013));
#15069=DIRECTION('',(0.,1.,0.));
#15070=DIRECTION('center_axis',(-0.894934361602026,0.,-0.446197813109807));
#15071=DIRECTION('ref_axis',(-0.446197813109807,0.,0.894934361602026));
#15072=DIRECTION('',(-0.446197813109807,0.,0.894934361602026));
#15073=DIRECTION('',(0.,1.,0.));
#15074=DIRECTION('center_axis',(-0.876026258834078,0.,-0.48226340710567));
#15075=DIRECTION('ref_axis',(-0.48226340710567,0.,0.876026258834078));
#15076=DIRECTION('',(-0.48226340710567,0.,0.876026258834078));
#15077=DIRECTION('',(0.,1.,0.));
#15078=DIRECTION('center_axis',(-0.855665491286185,0.,-0.517529290979719));
#15079=DIRECTION('ref_axis',(-0.517529290979719,0.,0.855665491286185));
#15080=DIRECTION('',(-0.517529290979719,0.,0.855665491286185));
#15081=DIRECTION('',(0.,1.,0.));
#15082=DIRECTION('center_axis',(-0.833885822067167,0.,-0.55193698531206));
#15083=DIRECTION('ref_axis',(-0.55193698531206,0.,0.833885822067167));
#15084=DIRECTION('',(-0.55193698531206,0.,0.833885822067167));
#15085=DIRECTION('',(0.,1.,0.));
#15086=DIRECTION('center_axis',(-0.810723367170213,0.,-0.585429433769939));
#15087=DIRECTION('ref_axis',(-0.585429433769939,0.,0.810723367170213));
#15088=DIRECTION('',(-0.58542943376994,0.,0.810723367170213));
#15089=DIRECTION('',(0.,1.,0.));
#15090=DIRECTION('center_axis',(0.601815023152048,0.,-0.798635510047293));
#15091=DIRECTION('ref_axis',(-0.798635510047293,0.,-0.601815023152048));
#15092=DIRECTION('',(-0.798635510047293,0.,-0.601815023152048));
#15093=DIRECTION('center_axis',(0.,1.,0.));
#15094=DIRECTION('ref_axis',(0.5,0.,-0.866025403784439));
#15095=DIRECTION('center_axis',(0.992546151641322,0.,-0.121869343405147));
#15096=DIRECTION('ref_axis',(-0.121869343405147,0.,-0.992546151641322));
#15097=DIRECTION('',(0.,1.,0.));
#15098=DIRECTION('',(-0.121869343405147,0.,-0.992546151641322));
#15099=DIRECTION('',(0.,1.,0.));
#15100=DIRECTION('',(0.121869343405147,0.,0.992546151641322));
#15101=DIRECTION('',(0.,1.,0.));
#15102=DIRECTION('center_axis',(-0.101635078182804,0.,-0.994821748296033));
#15103=DIRECTION('ref_axis',(-0.994821748296033,0.,0.101635078182804));
#15104=DIRECTION('',(0.,1.,0.));
#15105=DIRECTION('',(-0.994821748296033,0.,0.101635078182804));
#15106=DIRECTION('center_axis',(-0.101635078182804,0.,-0.994821748296033));
#15107=DIRECTION('ref_axis',(-0.994821748296033,0.,0.101635078182804));
#15108=DIRECTION('',(0.994821748296033,0.,-0.101635078182804));
#15109=DIRECTION('',(0.,1.,0.));
#15110=DIRECTION('center_axis',(-0.0610485395348574,0.,-0.998134798421867));
#15111=DIRECTION('ref_axis',(-0.998134798421867,0.,0.0610485395348574));
#15112=DIRECTION('',(0.,1.,0.));
#15113=DIRECTION('',(-0.998134798421867,0.,0.0610485395348574));
#15114=DIRECTION('center_axis',(-0.0203607675478923,0.,-0.999792698085389));
#15115=DIRECTION('ref_axis',(-0.999792698085389,0.,0.0203607675478923));
#15116=DIRECTION('',(0.,1.,0.));
#15117=DIRECTION('',(-0.999792698085389,0.,0.0203607675478923));
#15118=DIRECTION('center_axis',(0.0203607675478936,0.,-0.999792698085388));
#15119=DIRECTION('ref_axis',(-0.999792698085388,0.,-0.0203607675478936));
#15120=DIRECTION('',(0.,1.,0.));
#15121=DIRECTION('',(-0.999792698085388,0.,-0.0203607675478936));
#15122=DIRECTION('center_axis',(0.0610485395348586,0.,-0.998134798421867));
#15123=DIRECTION('ref_axis',(-0.998134798421867,0.,-0.0610485395348586));
#15124=DIRECTION('',(0.,1.,0.));
#15125=DIRECTION('',(-0.998134798421867,0.,-0.0610485395348586));
#15126=DIRECTION('center_axis',(0.101635078182805,0.,-0.994821748296033));
#15127=DIRECTION('ref_axis',(-0.994821748296033,0.,-0.101635078182805));
#15128=DIRECTION('',(0.,-1.,0.));
#15129=DIRECTION('',(-0.994821748296033,0.,-0.101635078182805));
#15130=DIRECTION('center_axis',(0.,-1.,0.));
#15131=DIRECTION('ref_axis',(1.,0.,6.10622663543836E-16));
#15132=DIRECTION('',(0.121869343405148,0.,-0.992546151641322));
#15133=DIRECTION('',(0.994821748296033,0.,0.101635078182805));
#15134=DIRECTION('',(0.998134798421867,0.,0.0610485395348586));
#15135=DIRECTION('',(0.999792698085388,0.,0.0203607675478936));
#15136=DIRECTION('',(0.999792698085389,0.,-0.0203607675478923));
#15137=DIRECTION('',(0.998134798421867,0.,-0.0610485395348574));
#15138=DIRECTION('',(-0.994821748296033,0.,0.1016350781828));
#15139=DIRECTION('',(-0.998134798421867,0.,0.0610485395348585));
#15140=DIRECTION('',(-0.999792698085389,0.,0.0203607675478921));
#15141=DIRECTION('',(-0.999792698085388,0.,-0.0203607675478933));
#15142=DIRECTION('',(-0.998134798421867,0.,-0.0610485395348597));
#15143=DIRECTION('',(-0.994821748296033,0.,-0.101635078182801));
#15144=DIRECTION('center_axis',(0.101635078182805,0.,-0.994821748296033));
#15145=DIRECTION('ref_axis',(-0.994821748296033,0.,-0.101635078182805));
#15146=DIRECTION('',(0.,1.,0.));
#15147=DIRECTION('',(0.,-1.,0.));
#15148=DIRECTION('center_axis',(0.0610485395348586,0.,-0.998134798421867));
#15149=DIRECTION('ref_axis',(-0.998134798421867,0.,-0.0610485395348586));
#15150=DIRECTION('',(0.,1.,0.));
#15151=DIRECTION('center_axis',(0.0203607675478936,0.,-0.999792698085388));
#15152=DIRECTION('ref_axis',(-0.999792698085388,0.,-0.0203607675478936));
#15153=DIRECTION('',(0.,1.,0.));
#15154=DIRECTION('center_axis',(-0.0203607675478923,0.,-0.999792698085389));
#15155=DIRECTION('ref_axis',(-0.999792698085389,0.,0.0203607675478923));
#15156=DIRECTION('',(0.,1.,0.));
#15157=DIRECTION('center_axis',(-0.0610485395348574,0.,-0.998134798421867));
#15158=DIRECTION('ref_axis',(-0.998134798421867,0.,0.0610485395348574));
#15159=DIRECTION('center_axis',(0.1016350781828,0.,0.994821748296033));
#15160=DIRECTION('ref_axis',(0.994821748296033,0.,-0.1016350781828));
#15161=DIRECTION('',(0.994821748296033,0.,-0.1016350781828));
#15162=DIRECTION('',(0.,1.,0.));
#15163=DIRECTION('center_axis',(0.0610485395348585,0.,0.998134798421867));
#15164=DIRECTION('ref_axis',(0.998134798421867,0.,-0.0610485395348585));
#15165=DIRECTION('',(0.998134798421867,0.,-0.0610485395348585));
#15166=DIRECTION('',(0.,1.,0.));
#15167=DIRECTION('center_axis',(0.0203607675478921,0.,0.999792698085389));
#15168=DIRECTION('ref_axis',(0.999792698085389,0.,-0.0203607675478921));
#15169=DIRECTION('',(0.999792698085389,0.,-0.0203607675478921));
#15170=DIRECTION('',(0.,1.,0.));
#15171=DIRECTION('center_axis',(-0.0203607675478933,0.,0.999792698085389));
#15172=DIRECTION('ref_axis',(0.999792698085388,0.,0.0203607675478933));
#15173=DIRECTION('',(0.999792698085388,0.,0.0203607675478933));
#15174=DIRECTION('',(0.,1.,0.));
#15175=DIRECTION('center_axis',(-0.0610485395348597,0.,0.998134798421867));
#15176=DIRECTION('ref_axis',(0.998134798421867,0.,0.0610485395348597));
#15177=DIRECTION('',(0.998134798421867,0.,0.0610485395348597));
#15178=DIRECTION('',(0.,1.,0.));
#15179=DIRECTION('center_axis',(-0.101635078182801,0.,0.994821748296033));
#15180=DIRECTION('ref_axis',(0.994821748296033,0.,0.101635078182801));
#15181=DIRECTION('',(0.994821748296033,0.,0.101635078182801));
#15182=DIRECTION('',(0.,1.,0.));
#15183=DIRECTION('center_axis',(-0.992546151641322,0.,-0.121869343405148));
#15184=DIRECTION('ref_axis',(-0.121869343405148,0.,0.992546151641322));
#15185=DIRECTION('',(-0.121869343405148,0.,0.992546151641322));
#15186=DIRECTION('center_axis',(0.,1.,0.));
#15187=DIRECTION('ref_axis',(-1.,0.,-6.10622663543836E-16));
#15188=DIRECTION('',(0.,0.,1.));
#15189=DIRECTION('',(1.,0.,0.));
#15190=DIRECTION('',(0.,0.,1.));
#15191=DIRECTION('',(1.,0.,0.));
#15192=DIRECTION('',(0.,0.,1.));
#15193=DIRECTION('',(1.,0.,0.));
#15194=DIRECTION('axis',(0.,0.,1.));
#15195=DIRECTION('refdir',(1.,0.,0.));
#15196=DIRECTION('center_axis',(0.,0.707106781186548,0.707106781186547));
#15197=DIRECTION('ref_axis',(1.,0.,0.));
#15198=DIRECTION('',(-1.96261557335472E-15,-0.707106781186547,0.707106781186548));
#15199=DIRECTION('',(1.,0.,0.));
#15200=DIRECTION('',(0.,0.707106781186547,-0.707106781186548));
#15201=DIRECTION('',(-1.,0.,0.));
#15202=DIRECTION('center_axis',(0.,0.,-1.));
#15203=DIRECTION('ref_axis',(0.,1.,0.));
#15204=DIRECTION('',(0.,0.707106781186548,0.707106781186548));
#15205=DIRECTION('center_axis',(0.,0.,-1.));
#15206=DIRECTION('ref_axis',(0.,1.,0.));
#15207=DIRECTION('center_axis',(0.,0.,1.));
#15208=DIRECTION('ref_axis',(0.,1.,0.));
#15209=DIRECTION('center_axis',(0.,-0.707106781186548,0.707106781186547));
#15210=DIRECTION('ref_axis',(1.,0.,0.));
#15211=DIRECTION('',(1.96261557335472E-15,0.707106781186547,0.707106781186548));
#15212=DIRECTION('',(-1.,0.,0.));
#15213=DIRECTION('',(1.,0.,0.));
#15214=DIRECTION('center_axis',(0.,0.,-1.));
#15215=DIRECTION('ref_axis',(0.,-1.,0.));
#15216=DIRECTION('center_axis',(0.,0.,-1.));
#15217=DIRECTION('ref_axis',(0.,-1.,0.));
#15218=DIRECTION('center_axis',(0.,0.,1.));
#15219=DIRECTION('ref_axis',(0.,-1.,0.));
#15220=DIRECTION('center_axis',(0.,0.,1.));
#15221=DIRECTION('ref_axis',(0.,1.,0.));
#15222=DIRECTION('',(0.,0.,1.));
#15223=DIRECTION('center_axis',(0.,0.,-1.));
#15224=DIRECTION('ref_axis',(0.,1.,0.));
#15225=DIRECTION('',(0.,0.,1.));
#15226=DIRECTION('center_axis',(0.,1.,0.));
#15227=DIRECTION('ref_axis',(-1.,0.,0.));
#15228=DIRECTION('',(0.,0.,1.));
#15229=DIRECTION('',(1.,0.,0.));
#15230=DIRECTION('center_axis',(0.,0.,1.));
#15231=DIRECTION('ref_axis',(1.,0.,0.));
#15232=DIRECTION('center_axis',(0.,0.707106781186548,-0.707106781186548));
#15233=DIRECTION('ref_axis',(-1.,0.,0.));
#15234=DIRECTION('',(1.96261557335472E-15,0.707106781186548,0.707106781186548));
#15235=DIRECTION('',(0.,-0.707106781186548,-0.707106781186548));
#15236=DIRECTION('',(-1.,0.,0.));
#15237=DIRECTION('center_axis',(0.,0.,1.));
#15238=DIRECTION('ref_axis',(0.,1.,0.));
#15239=DIRECTION('',(0.,-0.707106781186548,0.707106781186547));
#15240=DIRECTION('center_axis',(0.,0.,1.));
#15241=DIRECTION('ref_axis',(0.,1.,0.));
#15242=DIRECTION('center_axis',(0.,-0.707106781186548,-0.707106781186548));
#15243=DIRECTION('ref_axis',(-1.,0.,0.));
#15244=DIRECTION('',(-1.96261557335472E-15,-0.707106781186548,0.707106781186548));
#15245=DIRECTION('',(-1.,0.,0.));
#15246=DIRECTION('',(1.,0.,0.));
#15247=DIRECTION('center_axis',(0.,0.,1.));
#15248=DIRECTION('ref_axis',(0.,-1.,0.));
#15249=DIRECTION('center_axis',(0.,0.,-1.));
#15250=DIRECTION('ref_axis',(0.,-1.,0.));
#15251=DIRECTION('center_axis',(0.,0.,1.));
#15252=DIRECTION('ref_axis',(0.,-1.,0.));
#15253=DIRECTION('center_axis',(0.,0.,1.));
#15254=DIRECTION('ref_axis',(0.,-1.,0.));
#15255=DIRECTION('',(0.,0.,1.));
#15256=DIRECTION('center_axis',(0.,0.,1.));
#15257=DIRECTION('ref_axis',(1.,0.,0.));
#15258=DIRECTION('center_axis',(0.,-1.,0.));
#15259=DIRECTION('ref_axis',(1.,0.,0.));
#15260=DIRECTION('axis',(0.,0.,1.));
#15261=DIRECTION('refdir',(1.,0.,0.));
#15262=DIRECTION('center_axis',(0.866025403784439,0.,-0.5));
#15263=DIRECTION('ref_axis',(0.5,0.,0.866025403784439));
#15264=DIRECTION('',(0.5,0.,0.866025403784439));
#15265=DIRECTION('',(0.,-1.,0.));
#15266=DIRECTION('',(0.5,0.,0.866025403784439));
#15267=DIRECTION('',(0.,-1.,0.));
#15268=DIRECTION('center_axis',(1.92296268638356E-16,0.,-1.));
#15269=DIRECTION('ref_axis',(1.,0.,1.92296268638356E-16));
#15270=DIRECTION('',(1.,0.,1.92296268638356E-16));
#15271=DIRECTION('',(0.,-1.,0.));
#15272=DIRECTION('',(1.,0.,1.92296268638356E-16));
#15273=DIRECTION('center_axis',(-0.866025403784439,0.,-0.5));
#15274=DIRECTION('ref_axis',(0.5,0.,-0.866025403784439));
#15275=DIRECTION('',(0.5,0.,-0.866025403784439));
#15276=DIRECTION('',(0.,-1.,0.));
#15277=DIRECTION('',(0.5,0.,-0.866025403784438));
#15278=DIRECTION('center_axis',(-0.866025403784439,0.,0.5));
#15279=DIRECTION('ref_axis',(-0.5,0.,-0.866025403784439));
#15280=DIRECTION('',(-0.5,0.,-0.866025403784439));
#15281=DIRECTION('',(0.,-1.,0.));
#15282=DIRECTION('',(-0.5,0.,-0.866025403784439));
#15283=DIRECTION('center_axis',(-1.92296268638356E-16,0.,1.));
#15284=DIRECTION('ref_axis',(-1.,0.,-1.92296268638356E-16));
#15285=DIRECTION('',(-1.,0.,-1.92296268638356E-16));
#15286=DIRECTION('',(0.,-1.,0.));
#15287=DIRECTION('',(-1.,0.,-1.92296268638356E-16));
#15288=DIRECTION('center_axis',(0.866025403784439,0.,0.5));
#15289=DIRECTION('ref_axis',(-0.5,0.,0.866025403784439));
#15290=DIRECTION('',(-0.5,0.,0.866025403784439));
#15291=DIRECTION('',(-0.5,0.,0.866025403784439));
#15292=DIRECTION('center_axis',(0.,-1.,0.));
#15293=DIRECTION('ref_axis',(0.,0.,-1.));
#15294=DIRECTION('center_axis',(0.,1.,0.));
#15295=DIRECTION('ref_axis',(0.,0.,1.));
#15296=DIRECTION('center_axis',(0.,-1.,0.));
#15297=DIRECTION('ref_axis',(1.,0.,0.));
#15298=DIRECTION('center_axis',(0.,-1.,0.));
#15299=DIRECTION('ref_axis',(1.,0.,0.));
#15300=DIRECTION('center_axis',(0.,-1.,0.));
#15301=DIRECTION('ref_axis',(1.,0.,0.));
#15302=DIRECTION('',(0.707106781186547,0.707106781186548,8.65956056235493E-17));
#15303=DIRECTION('center_axis',(0.,-1.,0.));
#15304=DIRECTION('ref_axis',(1.,0.,0.));
#15305=DIRECTION('center_axis',(0.,1.,0.));
#15306=DIRECTION('ref_axis',(1.,0.,0.));
#15307=DIRECTION('',(0.,1.,0.));
#15308=DIRECTION('center_axis',(0.,1.,0.));
#15309=DIRECTION('ref_axis',(1.,0.,0.));
#15310=DIRECTION('center_axis',(0.,-1.,0.));
#15311=DIRECTION('ref_axis',(1.,0.,0.));
#15312=DIRECTION('',(-0.707106781186547,0.707106781186548,-8.65956056235493E-17));
#15313=DIRECTION('center_axis',(0.,-1.,0.));
#15314=DIRECTION('ref_axis',(0.,0.,-1.));
#15315=DIRECTION('axis',(0.,0.,1.));
#15316=DIRECTION('refdir',(1.,0.,0.));
#15317=DIRECTION('center_axis',(0.,1.,0.));
#15318=DIRECTION('ref_axis',(0.,0.,1.));
#15319=DIRECTION('center_axis',(0.,-1.,0.));
#15320=DIRECTION('ref_axis',(1.,0.,0.));
#15321=DIRECTION('center_axis',(0.,-1.,0.));
#15322=DIRECTION('ref_axis',(1.,0.,0.));
#15323=DIRECTION('center_axis',(0.,-1.,0.));
#15324=DIRECTION('ref_axis',(1.,0.,0.));
#15325=DIRECTION('',(0.707106781186547,0.707106781186548,8.65956056235493E-17));
#15326=DIRECTION('center_axis',(0.,-1.,0.));
#15327=DIRECTION('ref_axis',(1.,0.,0.));
#15328=DIRECTION('center_axis',(0.,-1.,0.));
#15329=DIRECTION('ref_axis',(1.,0.,0.));
#15330=DIRECTION('',(0.,1.,0.));
#15331=DIRECTION('center_axis',(0.,1.,0.));
#15332=DIRECTION('ref_axis',(1.,0.,0.));
#15333=DIRECTION('center_axis',(0.,-1.,0.));
#15334=DIRECTION('ref_axis',(1.,0.,0.));
#15335=DIRECTION('',(-0.707106781186547,0.707106781186548,-8.65956056235493E-17));
#15336=DIRECTION('center_axis',(0.,-1.,0.));
#15337=DIRECTION('ref_axis',(0.,0.,-1.));
#15338=DIRECTION('center_axis',(0.,-1.,0.));
#15339=DIRECTION('ref_axis',(1.,0.,0.));
#15340=DIRECTION('center_axis',(0.,1.,0.));
#15341=DIRECTION('ref_axis',(1.,0.,0.));
#15342=DIRECTION('center_axis',(0.,1.,0.));
#15343=DIRECTION('ref_axis',(1.,0.,0.));
#15344=DIRECTION('',(-0.447213595499958,0.894427190999916,-5.47678698264203E-17));
#15345=DIRECTION('center_axis',(0.,-1.,0.));
#15346=DIRECTION('ref_axis',(1.,0.,0.));
#15347=DIRECTION('center_axis',(0.,1.,0.));
#15348=DIRECTION('ref_axis',(1.,0.,0.));
#15349=DIRECTION('',(0.,1.,0.));
#15350=DIRECTION('center_axis',(0.,1.,0.));
#15351=DIRECTION('ref_axis',(1.,0.,0.));
#15352=DIRECTION('center_axis',(0.,-1.,0.));
#15353=DIRECTION('ref_axis',(1.,0.,0.));
#15354=DIRECTION('',(-0.707106781186547,0.707106781186548,-8.65956056235493E-17));
#15355=DIRECTION('center_axis',(0.,-1.,0.));
#15356=DIRECTION('ref_axis',(0.,0.,-1.));
#15357=DIRECTION('center_axis',(0.866025403784439,0.,-0.5));
#15358=DIRECTION('ref_axis',(0.5,0.,0.866025403784439));
#15359=DIRECTION('',(-0.5,0.,-0.866025403784439));
#15360=DIRECTION('',(0.,-1.,0.));
#15361=DIRECTION('',(0.5,0.,0.866025403784439));
#15362=DIRECTION('',(0.,-1.,0.));
#15363=DIRECTION('center_axis',(1.60246890531964E-16,0.,-1.));
#15364=DIRECTION('ref_axis',(1.,0.,1.60246890531964E-16));
#15365=DIRECTION('',(-1.,0.,-1.60246890531964E-16));
#15366=DIRECTION('',(0.,-1.,0.));
#15367=DIRECTION('',(1.,0.,1.60246890531964E-16));
#15368=DIRECTION('center_axis',(-0.866025403784439,0.,-0.5));
#15369=DIRECTION('ref_axis',(0.5,0.,-0.866025403784439));
#15370=DIRECTION('',(-0.5,0.,0.866025403784439));
#15371=DIRECTION('',(0.,-1.,0.));
#15372=DIRECTION('',(0.5,0.,-0.866025403784439));
#15373=DIRECTION('center_axis',(-0.866025403784439,0.,0.5));
#15374=DIRECTION('ref_axis',(-0.5,0.,-0.866025403784439));
#15375=DIRECTION('',(0.5,0.,0.866025403784439));
#15376=DIRECTION('',(0.,-1.,0.));
#15377=DIRECTION('',(-0.5,0.,-0.866025403784439));
#15378=DIRECTION('center_axis',(-1.60246890531964E-16,0.,1.));
#15379=DIRECTION('ref_axis',(-1.,0.,-1.60246890531964E-16));
#15380=DIRECTION('',(1.,0.,1.60246890531964E-16));
#15381=DIRECTION('',(0.,-1.,0.));
#15382=DIRECTION('',(-1.,0.,-1.60246890531964E-16));
#15383=DIRECTION('center_axis',(0.866025403784439,0.,0.5));
#15384=DIRECTION('ref_axis',(-0.5,0.,0.866025403784439));
#15385=DIRECTION('',(0.5,0.,-0.866025403784439));
#15386=DIRECTION('',(-0.5,0.,0.866025403784439));
#15387=DIRECTION('center_axis',(0.,1.,0.));
#15388=DIRECTION('ref_axis',(1.,0.,0.));
#15389=DIRECTION('center_axis',(0.,-1.,0.));
#15390=DIRECTION('ref_axis',(0.,0.,-1.));
#15391=DIRECTION('',(0.,0.,1.));
#15392=DIRECTION('',(1.,0.,0.));
#15393=DIRECTION('',(0.,0.,1.));
#15394=DIRECTION('',(1.,0.,0.));
#15395=DIRECTION('',(0.,0.,1.));
#15396=DIRECTION('',(1.,0.,0.));
#15397=DIRECTION('',(0.,0.,1.));
#15398=DIRECTION('',(1.,0.,0.));
#15399=DIRECTION('',(0.,0.,1.));
#15400=DIRECTION('',(1.,0.,0.));
#15401=DIRECTION('',(0.,0.,1.));
#15402=DIRECTION('',(1.,0.,0.));
#15403=DIRECTION('',(0.,0.,1.));
#15404=DIRECTION('',(1.,0.,0.));
#15405=DIRECTION('',(0.,-1.,2.22044604925031E-16));
#15406=DIRECTION('',(1.,0.,0.));
#15407=DIRECTION('',(0.,0.,1.));
#15408=DIRECTION('',(1.,0.,0.));
#15409=DIRECTION('',(0.,-1.,0.));
#15410=DIRECTION('',(1.,0.,0.));
#15411=DIRECTION('',(0.,-1.,0.));
#15412=DIRECTION('',(0.5,0.,-0.866025403784439));
#15413=DIRECTION('',(8.65956056235493E-17,-8.65956056235493E-17,-1.));
#15414=DIRECTION('',(2.22044604925031E-16,1.,-8.65956056235494E-17));
#15415=DIRECTION('',(0.,-1.,2.22044604925031E-16));
#15416=DIRECTION('',(1.,0.,0.));
#15417=DIRECTION('',(0.,-1.,2.22044604925031E-16));
#15418=DIRECTION('',(1.,0.,0.));
#15419=DIRECTION('',(0.,-1.,2.22044604925031E-16));
#15420=DIRECTION('',(1.,0.,0.));
#15421=DIRECTION('',(0.,0.,1.));
#15422=DIRECTION('',(1.,0.,0.));
#15423=DIRECTION('',(0.,0.,1.));
#15424=DIRECTION('',(1.,0.,0.));
#15425=DIRECTION('',(0.,0.,1.));
#15426=DIRECTION('',(1.,0.,0.));
#15427=CARTESIAN_POINT('',(0.,0.,0.));
#15428=CARTESIAN_POINT('',(0.,0.,0.));
#15429=CARTESIAN_POINT('',(0.,0.,0.));
#15430=CARTESIAN_POINT('Origin',(-2.8,-9.,-0.1));
#15431=CARTESIAN_POINT('',(-3.01,-9.,0.));
#15432=CARTESIAN_POINT('Origin',(-2.8,-9.,0.));
#15433=CARTESIAN_POINT('',(-3.01,-9.,1.2));
#15434=CARTESIAN_POINT('',(-3.01,-9.,-0.1));
#15435=CARTESIAN_POINT('Origin',(-2.8,-9.,1.2));
#15436=CARTESIAN_POINT('Origin',(2.8,-9.,-0.1));
#15437=CARTESIAN_POINT('',(2.59,-9.,0.));
#15438=CARTESIAN_POINT('Origin',(2.8,-9.,0.));
#15439=CARTESIAN_POINT('',(2.59,-9.,1.2));
#15440=CARTESIAN_POINT('',(2.59,-9.,-0.1));
#15441=CARTESIAN_POINT('Origin',(2.8,-9.,1.2));
#15442=CARTESIAN_POINT('Origin',(4.75,2.,-0.1));
#15443=CARTESIAN_POINT('',(4.41,2.,0.));
#15444=CARTESIAN_POINT('Origin',(4.75,2.,0.));
#15445=CARTESIAN_POINT('',(4.41,2.,1.2));
#15446=CARTESIAN_POINT('',(4.41,2.,-0.1));
#15447=CARTESIAN_POINT('Origin',(4.75,2.,1.2));
#15448=CARTESIAN_POINT('Origin',(-4.75,18.,-0.1));
#15449=CARTESIAN_POINT('',(-5.09,18.,0.));
#15450=CARTESIAN_POINT('Origin',(-4.75,18.,0.));
#15451=CARTESIAN_POINT('',(-5.09,18.,1.2));
#15452=CARTESIAN_POINT('',(-5.09,18.,-0.1));
#15453=CARTESIAN_POINT('Origin',(-4.75,18.,1.2));
#15454=CARTESIAN_POINT('Origin',(-4.75,2.,-0.1));
#15455=CARTESIAN_POINT('',(-5.09,2.,0.));
#15456=CARTESIAN_POINT('Origin',(-4.75,2.,0.));
#15457=CARTESIAN_POINT('',(-5.09,2.,1.2));
#15458=CARTESIAN_POINT('',(-5.09,2.,-0.1));
#15459=CARTESIAN_POINT('Origin',(-4.75,2.,1.2));
#15460=CARTESIAN_POINT('Origin',(4.75,18.,-0.1));
#15461=CARTESIAN_POINT('',(4.41,18.,0.));
#15462=CARTESIAN_POINT('Origin',(4.75,18.,0.));
#15463=CARTESIAN_POINT('',(4.41,18.,1.2));
#15464=CARTESIAN_POINT('',(4.41,18.,-0.1));
#15465=CARTESIAN_POINT('Origin',(4.75,18.,1.2));
#15466=CARTESIAN_POINT('Origin',(7.,25.,0.));
#15467=CARTESIAN_POINT('',(7.,25.,0.));
#15468=CARTESIAN_POINT('',(-7.,25.,0.));
#15469=CARTESIAN_POINT('',(7.,25.,0.));
#15470=CARTESIAN_POINT('',(-7.,25.,1.2));
#15471=CARTESIAN_POINT('',(-7.,25.,0.));
#15472=CARTESIAN_POINT('',(7.,25.,1.2));
#15473=CARTESIAN_POINT('',(7.,25.,1.2));
#15474=CARTESIAN_POINT('',(7.,25.,0.));
#15475=CARTESIAN_POINT('Origin',(7.,-12.5,0.));
#15476=CARTESIAN_POINT('',(7.,-12.5,0.));
#15477=CARTESIAN_POINT('',(7.,-12.5,0.));
#15478=CARTESIAN_POINT('',(7.,-12.5,1.2));
#15479=CARTESIAN_POINT('',(7.,-12.5,1.2));
#15480=CARTESIAN_POINT('',(7.,-12.5,0.));
#15481=CARTESIAN_POINT('Origin',(-7.,-12.5,0.));
#15482=CARTESIAN_POINT('',(-7.,-12.5,0.));
#15483=CARTESIAN_POINT('',(-7.,-12.5,0.));
#15484=CARTESIAN_POINT('',(-7.,-12.5,1.2));
#15485=CARTESIAN_POINT('',(-7.,-12.5,1.2));
#15486=CARTESIAN_POINT('',(-7.,-12.5,0.));
#15487=CARTESIAN_POINT('Origin',(-7.,25.,0.));
#15488=CARTESIAN_POINT('',(-7.,25.,0.));
#15489=CARTESIAN_POINT('',(-7.,25.,1.2));
#15490=CARTESIAN_POINT('Origin',(0.,6.25,1.2));
#15491=CARTESIAN_POINT('Origin',(0.,6.25,0.));
#15492=CARTESIAN_POINT('',(0.,0.,0.));
#15493=CARTESIAN_POINT('Origin',(7.,-11.5,-0.5));
#15494=CARTESIAN_POINT('',(7.,-11.5,-0.5));
#15495=CARTESIAN_POINT('',(-7.,-11.5,-0.5));
#15496=CARTESIAN_POINT('',(7.,-11.5,-0.5));
#15497=CARTESIAN_POINT('',(-7.,-11.5,0.));
#15498=CARTESIAN_POINT('',(-7.,-11.5,-0.5));
#15499=CARTESIAN_POINT('',(7.,-11.5,0.));
#15500=CARTESIAN_POINT('',(7.,-11.5,0.));
#15501=CARTESIAN_POINT('',(7.,-11.5,-0.5));
#15502=CARTESIAN_POINT('Origin',(7.,-12.5,-0.5));
#15503=CARTESIAN_POINT('',(7.,-12.5,-0.5));
#15504=CARTESIAN_POINT('',(7.,-12.5,-0.5));
#15505=CARTESIAN_POINT('',(7.,-12.5,0.));
#15506=CARTESIAN_POINT('',(7.,-12.5,0.));
#15507=CARTESIAN_POINT('',(7.,-12.5,-0.5));
#15508=CARTESIAN_POINT('Origin',(-7.,-12.5,-0.5));
#15509=CARTESIAN_POINT('',(-7.,-12.5,-0.5));
#15510=CARTESIAN_POINT('',(-7.,-12.5,-0.5));
#15511=CARTESIAN_POINT('',(-7.,-12.5,0.));
#15512=CARTESIAN_POINT('',(-7.,-12.5,0.));
#15513=CARTESIAN_POINT('',(-7.,-12.5,-0.5));
#15514=CARTESIAN_POINT('Origin',(-7.,-11.5,-0.5));
#15515=CARTESIAN_POINT('',(-7.,-11.5,-0.5));
#15516=CARTESIAN_POINT('',(-7.,-11.5,0.));
#15517=CARTESIAN_POINT('Origin',(0.,-12.,0.));
#15518=CARTESIAN_POINT('Origin',(0.,-12.,-0.5));
#15519=CARTESIAN_POINT('',(0.,0.,0.));
#15520=CARTESIAN_POINT('Origin',(7.,25.,-0.5));
#15521=CARTESIAN_POINT('',(7.,25.,-0.5));
#15522=CARTESIAN_POINT('',(-7.,25.,-0.5));
#15523=CARTESIAN_POINT('',(7.,25.,-0.5));
#15524=CARTESIAN_POINT('',(-7.,25.,0.));
#15525=CARTESIAN_POINT('',(-7.,25.,-0.5));
#15526=CARTESIAN_POINT('',(7.,25.,0.));
#15527=CARTESIAN_POINT('',(7.,25.,0.));
#15528=CARTESIAN_POINT('',(7.,25.,-0.5));
#15529=CARTESIAN_POINT('Origin',(7.,24.,-0.5));
#15530=CARTESIAN_POINT('',(7.,24.,-0.5));
#15531=CARTESIAN_POINT('',(7.,24.,-0.5));
#15532=CARTESIAN_POINT('',(7.,24.,0.));
#15533=CARTESIAN_POINT('',(7.,24.,0.));
#15534=CARTESIAN_POINT('',(7.,24.,-0.5));
#15535=CARTESIAN_POINT('Origin',(-7.,24.,-0.5));
#15536=CARTESIAN_POINT('',(-7.,24.,-0.5));
#15537=CARTESIAN_POINT('',(-7.,24.,-0.5));
#15538=CARTESIAN_POINT('',(-7.,24.,0.));
#15539=CARTESIAN_POINT('',(-7.,24.,0.));
#15540=CARTESIAN_POINT('',(-7.,24.,-0.5));
#15541=CARTESIAN_POINT('Origin',(-7.,25.,-0.5));
#15542=CARTESIAN_POINT('',(-7.,25.,-0.5));
#15543=CARTESIAN_POINT('',(-7.,25.,0.));
#15544=CARTESIAN_POINT('Origin',(0.,24.5,0.));
#15545=CARTESIAN_POINT('Origin',(0.,24.5,-0.5));
#15546=CARTESIAN_POINT('',(0.,0.,0.));
#15547=CARTESIAN_POINT('Origin',(-4.75,2.,1.2));
#15548=CARTESIAN_POINT('',(-5.175,2.,2.4));
#15549=CARTESIAN_POINT('Origin',(-4.75,2.,2.4));
#15550=CARTESIAN_POINT('',(-5.175,2.,1.2));
#15551=CARTESIAN_POINT('',(-5.175,2.,1.2));
#15552=CARTESIAN_POINT('Origin',(-4.75,2.,1.2));
#15553=CARTESIAN_POINT('Origin',(-4.75,2.,1.2));
#15554=CARTESIAN_POINT('',(-5.395,2.,2.4));
#15555=CARTESIAN_POINT('Origin',(-4.75,2.,2.4));
#15556=CARTESIAN_POINT('',(-5.395,2.,1.2));
#15557=CARTESIAN_POINT('',(-5.395,2.,1.2));
#15558=CARTESIAN_POINT('Origin',(-4.75,2.,1.2));
#15559=CARTESIAN_POINT('Origin',(-4.75,2.,2.4));
#15560=CARTESIAN_POINT('Origin',(-4.75,2.,1.2));
#15561=CARTESIAN_POINT('',(0.,0.,0.));
#15562=CARTESIAN_POINT('Origin',(4.75,2.,1.2));
#15563=CARTESIAN_POINT('',(4.325,2.,2.4));
#15564=CARTESIAN_POINT('Origin',(4.75,2.,2.4));
#15565=CARTESIAN_POINT('',(4.325,2.,1.2));
#15566=CARTESIAN_POINT('',(4.325,2.,1.2));
#15567=CARTESIAN_POINT('Origin',(4.75,2.,1.2));
#15568=CARTESIAN_POINT('Origin',(4.75,2.,1.2));
#15569=CARTESIAN_POINT('',(4.105,2.,2.4));
#15570=CARTESIAN_POINT('Origin',(4.75,2.,2.4));
#15571=CARTESIAN_POINT('',(4.105,2.,1.2));
#15572=CARTESIAN_POINT('',(4.105,2.,1.2));
#15573=CARTESIAN_POINT('Origin',(4.75,2.,1.2));
#15574=CARTESIAN_POINT('Origin',(4.75,2.,2.4));
#15575=CARTESIAN_POINT('Origin',(4.75,2.,1.2));
#15576=CARTESIAN_POINT('',(0.,0.,0.));
#15577=CARTESIAN_POINT('Origin',(-4.75,18.,1.2));
#15578=CARTESIAN_POINT('',(-5.175,18.,2.4));
#15579=CARTESIAN_POINT('Origin',(-4.75,18.,2.4));
#15580=CARTESIAN_POINT('',(-5.175,18.,1.2));
#15581=CARTESIAN_POINT('',(-5.175,18.,1.2));
#15582=CARTESIAN_POINT('Origin',(-4.75,18.,1.2));
#15583=CARTESIAN_POINT('Origin',(-4.75,18.,1.2));
#15584=CARTESIAN_POINT('',(-5.395,18.,2.4));
#15585=CARTESIAN_POINT('Origin',(-4.75,18.,2.4));
#15586=CARTESIAN_POINT('',(-5.395,18.,1.2));
#15587=CARTESIAN_POINT('',(-5.395,18.,1.2));
#15588=CARTESIAN_POINT('Origin',(-4.75,18.,1.2));
#15589=CARTESIAN_POINT('Origin',(-4.75,18.,2.4));
#15590=CARTESIAN_POINT('Origin',(-4.75,18.,1.2));
#15591=CARTESIAN_POINT('',(0.,0.,0.));
#15592=CARTESIAN_POINT('Origin',(4.75,18.,1.2));
#15593=CARTESIAN_POINT('',(4.325,18.,2.4));
#15594=CARTESIAN_POINT('Origin',(4.75,18.,2.4));
#15595=CARTESIAN_POINT('',(4.325,18.,1.2));
#15596=CARTESIAN_POINT('',(4.325,18.,1.2));
#15597=CARTESIAN_POINT('Origin',(4.75,18.,1.2));
#15598=CARTESIAN_POINT('Origin',(4.75,18.,1.2));
#15599=CARTESIAN_POINT('',(4.105,18.,2.4));
#15600=CARTESIAN_POINT('Origin',(4.75,18.,2.4));
#15601=CARTESIAN_POINT('',(4.105,18.,1.2));
#15602=CARTESIAN_POINT('',(4.105,18.,1.2));
#15603=CARTESIAN_POINT('Origin',(4.75,18.,1.2));
#15604=CARTESIAN_POINT('Origin',(4.75,18.,2.4));
#15605=CARTESIAN_POINT('Origin',(4.75,18.,1.2));
#15606=CARTESIAN_POINT('',(0.,0.,0.));
#15607=CARTESIAN_POINT('Origin',(1.55,-7.7,2.67));
#15608=CARTESIAN_POINT('',(1.38,-7.6,2.67));
#15609=CARTESIAN_POINT('Origin',(1.55,-7.6,2.67));
#15610=CARTESIAN_POINT('',(1.38,-7.,2.67));
#15611=CARTESIAN_POINT('',(1.38,-7.7,2.67));
#15612=CARTESIAN_POINT('Origin',(1.55,-7.,2.67));
#15613=CARTESIAN_POINT('Origin',(-1.55,-7.7,5.77));
#15614=CARTESIAN_POINT('',(-1.72,-7.6,5.77));
#15615=CARTESIAN_POINT('Origin',(-1.55,-7.6,5.77));
#15616=CARTESIAN_POINT('',(-1.72,-7.,5.77));
#15617=CARTESIAN_POINT('',(-1.72,-7.7,5.77));
#15618=CARTESIAN_POINT('Origin',(-1.55,-7.,5.77));
#15619=CARTESIAN_POINT('Origin',(-1.55,-7.7,2.67));
#15620=CARTESIAN_POINT('',(-1.72,-7.6,2.67));
#15621=CARTESIAN_POINT('Origin',(-1.55,-7.6,2.67));
#15622=CARTESIAN_POINT('',(-1.72,-7.,2.67));
#15623=CARTESIAN_POINT('',(-1.72,-7.7,2.67));
#15624=CARTESIAN_POINT('Origin',(-1.55,-7.,2.67));
#15625=CARTESIAN_POINT('Origin',(1.55,-7.7,5.77));
#15626=CARTESIAN_POINT('',(1.38,-7.6,5.77));
#15627=CARTESIAN_POINT('Origin',(1.55,-7.6,5.77));
#15628=CARTESIAN_POINT('',(1.38,-7.,5.77));
#15629=CARTESIAN_POINT('',(1.38,-7.7,5.77));
#15630=CARTESIAN_POINT('Origin',(1.55,-7.,5.77));
#15631=CARTESIAN_POINT('Origin',(0.,-7.7,4.22));
#15632=CARTESIAN_POINT('',(-1.11,-7.6,4.22));
#15633=CARTESIAN_POINT('Origin',(0.,-7.6,4.22));
#15634=CARTESIAN_POINT('',(-1.11,-7.,4.22));
#15635=CARTESIAN_POINT('',(-1.11,-7.7,4.22));
#15636=CARTESIAN_POINT('Origin',(0.,-7.,4.22));
#15637=CARTESIAN_POINT('Origin',(-2.8,-9.,1.1));
#15638=CARTESIAN_POINT('',(-3.075,-9.,1.2));
#15639=CARTESIAN_POINT('Origin',(-2.8,-9.,1.2));
#15640=CARTESIAN_POINT('',(-3.075,-9.,2.));
#15641=CARTESIAN_POINT('',(-3.075,-9.,1.1));
#15642=CARTESIAN_POINT('Origin',(-2.8,-9.,2.));
#15643=CARTESIAN_POINT('Origin',(2.8,-9.,1.1));
#15644=CARTESIAN_POINT('',(2.525,-9.,1.2));
#15645=CARTESIAN_POINT('Origin',(2.8,-9.,1.2));
#15646=CARTESIAN_POINT('',(2.525,-9.,2.));
#15647=CARTESIAN_POINT('',(2.525,-9.,1.1));
#15648=CARTESIAN_POINT('Origin',(2.8,-9.,2.));
#15649=CARTESIAN_POINT('Origin',(-3.5,-10.,2.));
#15650=CARTESIAN_POINT('',(-3.5,-7.6,2.));
#15651=CARTESIAN_POINT('',(3.5,-7.6,2.));
#15652=CARTESIAN_POINT('',(-3.5,-7.6,2.));
#15653=CARTESIAN_POINT('',(-3.5,-10.,2.));
#15654=CARTESIAN_POINT('',(-3.5,-10.,2.));
#15655=CARTESIAN_POINT('',(3.5,-10.,2.));
#15656=CARTESIAN_POINT('',(3.5,-10.,2.));
#15657=CARTESIAN_POINT('',(3.5,-10.,2.));
#15658=CARTESIAN_POINT('Origin',(0.,-10.,1.6));
#15659=CARTESIAN_POINT('',(-3.5,-10.,1.2));
#15660=CARTESIAN_POINT('',(-3.5,-10.,2.));
#15661=CARTESIAN_POINT('',(3.5,-10.,1.2));
#15662=CARTESIAN_POINT('',(-3.5,-10.,1.2));
#15663=CARTESIAN_POINT('',(3.5,-10.,1.2));
#15664=CARTESIAN_POINT('Origin',(3.5,-7.,1.2));
#15665=CARTESIAN_POINT('',(-3.5,-7.,1.2));
#15666=CARTESIAN_POINT('',(-3.5,-7.,7.5));
#15667=CARTESIAN_POINT('',(-3.5,-7.,1.2));
#15668=CARTESIAN_POINT('',(3.5,-7.,7.5));
#15669=CARTESIAN_POINT('',(3.5,-7.,7.5));
#15670=CARTESIAN_POINT('',(3.5,-7.,1.2));
#15671=CARTESIAN_POINT('',(3.5,-7.,1.2));
#15672=CARTESIAN_POINT('',(3.5,-7.,1.2));
#15673=CARTESIAN_POINT('Origin',(-3.5,-7.,1.2));
#15674=CARTESIAN_POINT('',(-3.5,-7.6,7.5));
#15675=CARTESIAN_POINT('',(-3.5,-7.6,1.2));
#15676=CARTESIAN_POINT('',(-3.5,-7.,7.5));
#15677=CARTESIAN_POINT('',(-3.5,-7.,1.2));
#15678=CARTESIAN_POINT('Origin',(3.5,-7.6,1.2));
#15679=CARTESIAN_POINT('',(3.5,-7.6,7.5));
#15680=CARTESIAN_POINT('',(3.5,-7.6,7.5));
#15681=CARTESIAN_POINT('',(3.5,-7.6,1.2));
#15682=CARTESIAN_POINT('',(3.5,-10.,1.2));
#15683=CARTESIAN_POINT('Origin',(-3.5,-7.6,1.2));
#15684=CARTESIAN_POINT('',(-3.5,-7.6,7.5));
#15685=CARTESIAN_POINT('Origin',(0.,-7.3,7.5));
#15686=CARTESIAN_POINT('Origin',(0.,-7.3,1.2));
#15687=CARTESIAN_POINT('',(0.,0.,0.));
#15688=CARTESIAN_POINT('Origin',(1.55,-8.2,2.67));
#15689=CARTESIAN_POINT('',(1.425,-8.2,2.67));
#15690=CARTESIAN_POINT('Origin',(1.55,-8.2,2.67));
#15691=CARTESIAN_POINT('',(1.425,-7.6,2.67));
#15692=CARTESIAN_POINT('',(1.425,-8.2,2.67));
#15693=CARTESIAN_POINT('Origin',(1.55,-7.6,2.67));
#15694=CARTESIAN_POINT('Origin',(1.55,-8.2,2.67));
#15695=CARTESIAN_POINT('Origin',(-1.55,-8.2,5.77));
#15696=CARTESIAN_POINT('',(-1.675,-8.2,5.77));
#15697=CARTESIAN_POINT('Origin',(-1.55,-8.2,5.77));
#15698=CARTESIAN_POINT('',(-1.675,-7.6,5.77));
#15699=CARTESIAN_POINT('',(-1.675,-8.2,5.77));
#15700=CARTESIAN_POINT('Origin',(-1.55,-7.6,5.77));
#15701=CARTESIAN_POINT('Origin',(-1.55,-8.2,5.77));
#15702=CARTESIAN_POINT('Origin',(-1.55,-8.2,2.67));
#15703=CARTESIAN_POINT('',(-1.675,-8.2,2.67));
#15704=CARTESIAN_POINT('Origin',(-1.55,-8.2,2.67));
#15705=CARTESIAN_POINT('',(-1.675,-7.6,2.67));
#15706=CARTESIAN_POINT('',(-1.675,-8.2,2.67));
#15707=CARTESIAN_POINT('Origin',(-1.55,-7.6,2.67));
#15708=CARTESIAN_POINT('Origin',(-1.55,-8.2,2.67));
#15709=CARTESIAN_POINT('Origin',(1.55,-8.2,5.77));
#15710=CARTESIAN_POINT('',(1.425,-8.2,5.77));
#15711=CARTESIAN_POINT('Origin',(1.55,-8.2,5.77));
#15712=CARTESIAN_POINT('',(1.425,-7.6,5.77));
#15713=CARTESIAN_POINT('',(1.425,-8.2,5.77));
#15714=CARTESIAN_POINT('Origin',(1.55,-7.6,5.77));
#15715=CARTESIAN_POINT('Origin',(1.55,-8.2,5.77));
#15716=CARTESIAN_POINT('Origin',(0.,-7.6,4.22));
#15717=CARTESIAN_POINT('',(-1.1,-7.4,4.22));
#15718=CARTESIAN_POINT('Origin',(0.,-7.4,4.22));
#15719=CARTESIAN_POINT('',(-1.1,-7.6,4.22));
#15720=CARTESIAN_POINT('',(-1.1,-7.6,4.22));
#15721=CARTESIAN_POINT('Origin',(0.,-7.6,4.22));
#15722=CARTESIAN_POINT('Origin',(0.,-7.4,4.22));
#15723=CARTESIAN_POINT('',(-0.26,-7.4,4.22));
#15724=CARTESIAN_POINT('Origin',(0.,-7.4,4.22));
#15725=CARTESIAN_POINT('Origin',(0.,-11.7,4.22));
#15726=CARTESIAN_POINT('',(-0.26,-11.6,4.22));
#15727=CARTESIAN_POINT('Origin',(0.,-11.6,4.22));
#15728=CARTESIAN_POINT('',(-0.26,-11.7,4.22));
#15729=CARTESIAN_POINT('Origin',(2.1,-7.6,2.12));
#15730=CARTESIAN_POINT('',(2.1,-7.6,2.12));
#15731=CARTESIAN_POINT('',(-2.1,-7.6,2.12));
#15732=CARTESIAN_POINT('',(2.1,-7.6,2.12));
#15733=CARTESIAN_POINT('',(-2.1,-7.6,6.32));
#15734=CARTESIAN_POINT('',(-2.1,-7.6,2.12));
#15735=CARTESIAN_POINT('',(2.1,-7.6,6.32));
#15736=CARTESIAN_POINT('',(2.1,-7.6,6.32));
#15737=CARTESIAN_POINT('',(2.1,-7.6,2.12));
#15738=CARTESIAN_POINT('Origin',(2.1,-11.6,2.12));
#15739=CARTESIAN_POINT('',(2.1,-11.6,2.12));
#15740=CARTESIAN_POINT('',(2.1,-11.6,2.12));
#15741=CARTESIAN_POINT('',(2.1,-11.6,6.32));
#15742=CARTESIAN_POINT('',(2.1,-11.6,6.32));
#15743=CARTESIAN_POINT('',(2.1,-11.6,2.12));
#15744=CARTESIAN_POINT('Origin',(-2.1,-11.6,2.12));
#15745=CARTESIAN_POINT('',(-2.1,-11.6,2.12));
#15746=CARTESIAN_POINT('',(-2.1,-11.6,2.12));
#15747=CARTESIAN_POINT('',(-2.1,-11.6,6.32));
#15748=CARTESIAN_POINT('',(-2.1,-11.6,6.32));
#15749=CARTESIAN_POINT('',(-2.1,-11.6,2.12));
#15750=CARTESIAN_POINT('Origin',(-2.1,-7.6,2.12));
#15751=CARTESIAN_POINT('',(-2.1,-7.6,2.12));
#15752=CARTESIAN_POINT('',(-2.1,-7.6,6.32));
#15753=CARTESIAN_POINT('Origin',(0.,-9.6,6.32));
#15754=CARTESIAN_POINT('Origin',(0.,-9.6,2.12));
#15755=CARTESIAN_POINT('',(0.,0.,0.));
#15756=CARTESIAN_POINT('Origin',(-1.69433756729741,-6.9,2.67));
#15757=CARTESIAN_POINT('',(-1.6221687836487,-6.7,2.795));
#15758=CARTESIAN_POINT('',(-1.69433756729741,-6.7,2.67));
#15759=CARTESIAN_POINT('',(-1.67629537138523,-6.7,2.70125));
#15760=CARTESIAN_POINT('',(-1.6221687836487,-6.9,2.795));
#15761=CARTESIAN_POINT('',(-1.6221687836487,-6.9,2.795));
#15762=CARTESIAN_POINT('',(-1.69433756729741,-6.9,2.67));
#15763=CARTESIAN_POINT('',(-1.6221687836487,-6.9,2.795));
#15764=CARTESIAN_POINT('',(-1.69433756729741,-6.9,2.67));
#15765=CARTESIAN_POINT('Origin',(-1.6221687836487,-6.9,2.545));
#15766=CARTESIAN_POINT('',(-1.6221687836487,-6.7,2.545));
#15767=CARTESIAN_POINT('',(-1.64021097956088,-6.7,2.57625));
#15768=CARTESIAN_POINT('',(-1.6221687836487,-6.9,2.545));
#15769=CARTESIAN_POINT('',(-1.69433756729741,-6.9,2.67));
#15770=CARTESIAN_POINT('',(-1.6221687836487,-6.9,2.545));
#15771=CARTESIAN_POINT('Origin',(-1.4778312163513,-6.9,2.545));
#15772=CARTESIAN_POINT('',(-1.4778312163513,-6.7,2.545));
#15773=CARTESIAN_POINT('',(-1.51391560817565,-6.7,2.545));
#15774=CARTESIAN_POINT('',(-1.4778312163513,-6.9,2.545));
#15775=CARTESIAN_POINT('',(-1.6221687836487,-6.9,2.545));
#15776=CARTESIAN_POINT('',(-1.4778312163513,-6.9,2.545));
#15777=CARTESIAN_POINT('Origin',(-1.40566243270259,-6.9,2.67));
#15778=CARTESIAN_POINT('',(-1.40566243270259,-6.7,2.67));
#15779=CARTESIAN_POINT('',(-1.42370462861477,-6.7,2.63875));
#15780=CARTESIAN_POINT('',(-1.40566243270259,-6.9,2.67));
#15781=CARTESIAN_POINT('',(-1.4778312163513,-6.9,2.545));
#15782=CARTESIAN_POINT('',(-1.40566243270259,-6.9,2.67));
#15783=CARTESIAN_POINT('Origin',(-1.4778312163513,-6.9,2.795));
#15784=CARTESIAN_POINT('',(-1.4778312163513,-6.7,2.795));
#15785=CARTESIAN_POINT('',(-1.45978902043912,-6.7,2.76375));
#15786=CARTESIAN_POINT('',(-1.4778312163513,-6.9,2.795));
#15787=CARTESIAN_POINT('',(-1.40566243270259,-6.9,2.67));
#15788=CARTESIAN_POINT('',(-1.4778312163513,-6.9,2.795));
#15789=CARTESIAN_POINT('Origin',(-1.6221687836487,-6.9,2.795));
#15790=CARTESIAN_POINT('',(-1.58608439182435,-6.7,2.795));
#15791=CARTESIAN_POINT('',(-1.4778312163513,-6.9,2.795));
#15792=CARTESIAN_POINT('Origin',(-1.55,-6.9,2.67));
#15793=CARTESIAN_POINT('Origin',(-1.55,-7.,2.67));
#15794=CARTESIAN_POINT('',(-1.825,-7.,2.67));
#15795=CARTESIAN_POINT('Origin',(-1.55,-7.,2.67));
#15796=CARTESIAN_POINT('',(-1.7,-7.,2.67));
#15797=CARTESIAN_POINT('Origin',(-1.55,-7.,2.67));
#15798=CARTESIAN_POINT('Origin',(-1.55,-7.,2.67));
#15799=CARTESIAN_POINT('',(-1.825,-6.7,2.67));
#15800=CARTESIAN_POINT('Origin',(-1.55,-6.7,2.67));
#15801=CARTESIAN_POINT('',(-1.825,-7.,2.67));
#15802=CARTESIAN_POINT('Origin',(-1.55,-6.7,2.67));
#15803=CARTESIAN_POINT('Origin',(-1.55,-8.,2.67));
#15804=CARTESIAN_POINT('',(-1.7,-8.,2.67));
#15805=CARTESIAN_POINT('',(-1.7,-8.,2.67));
#15806=CARTESIAN_POINT('Origin',(-1.55,-8.,2.67));
#15807=CARTESIAN_POINT('Origin',(-1.55,-8.,2.67));
#15808=CARTESIAN_POINT('',(0.,0.,0.));
#15809=CARTESIAN_POINT('Origin',(-1.69433756729741,-6.9,5.77));
#15810=CARTESIAN_POINT('',(-1.6221687836487,-6.7,5.895));
#15811=CARTESIAN_POINT('',(-1.69433756729741,-6.7,5.77));
#15812=CARTESIAN_POINT('',(-1.67629537138523,-6.7,5.80125));
#15813=CARTESIAN_POINT('',(-1.6221687836487,-6.9,5.895));
#15814=CARTESIAN_POINT('',(-1.6221687836487,-6.9,5.895));
#15815=CARTESIAN_POINT('',(-1.69433756729741,-6.9,5.77));
#15816=CARTESIAN_POINT('',(-1.6221687836487,-6.9,5.895));
#15817=CARTESIAN_POINT('',(-1.69433756729741,-6.9,5.77));
#15818=CARTESIAN_POINT('Origin',(-1.6221687836487,-6.9,5.645));
#15819=CARTESIAN_POINT('',(-1.6221687836487,-6.7,5.645));
#15820=CARTESIAN_POINT('',(-1.64021097956088,-6.7,5.67625));
#15821=CARTESIAN_POINT('',(-1.6221687836487,-6.9,5.645));
#15822=CARTESIAN_POINT('',(-1.69433756729741,-6.9,5.77));
#15823=CARTESIAN_POINT('',(-1.6221687836487,-6.9,5.645));
#15824=CARTESIAN_POINT('Origin',(-1.4778312163513,-6.9,5.645));
#15825=CARTESIAN_POINT('',(-1.4778312163513,-6.7,5.645));
#15826=CARTESIAN_POINT('',(-1.51391560817565,-6.7,5.645));
#15827=CARTESIAN_POINT('',(-1.4778312163513,-6.9,5.645));
#15828=CARTESIAN_POINT('',(-1.6221687836487,-6.9,5.645));
#15829=CARTESIAN_POINT('',(-1.4778312163513,-6.9,5.645));
#15830=CARTESIAN_POINT('Origin',(-1.40566243270259,-6.9,5.77));
#15831=CARTESIAN_POINT('',(-1.40566243270259,-6.7,5.77));
#15832=CARTESIAN_POINT('',(-1.42370462861477,-6.7,5.73875));
#15833=CARTESIAN_POINT('',(-1.40566243270259,-6.9,5.77));
#15834=CARTESIAN_POINT('',(-1.4778312163513,-6.9,5.645));
#15835=CARTESIAN_POINT('',(-1.40566243270259,-6.9,5.77));
#15836=CARTESIAN_POINT('Origin',(-1.4778312163513,-6.9,5.895));
#15837=CARTESIAN_POINT('',(-1.4778312163513,-6.7,5.895));
#15838=CARTESIAN_POINT('',(-1.45978902043912,-6.7,5.86375));
#15839=CARTESIAN_POINT('',(-1.4778312163513,-6.9,5.895));
#15840=CARTESIAN_POINT('',(-1.40566243270259,-6.9,5.77));
#15841=CARTESIAN_POINT('',(-1.4778312163513,-6.9,5.895));
#15842=CARTESIAN_POINT('Origin',(-1.6221687836487,-6.9,5.895));
#15843=CARTESIAN_POINT('',(-1.58608439182435,-6.7,5.895));
#15844=CARTESIAN_POINT('',(-1.4778312163513,-6.9,5.895));
#15845=CARTESIAN_POINT('Origin',(-1.55,-6.9,5.77));
#15846=CARTESIAN_POINT('Origin',(-1.55,-7.,5.77));
#15847=CARTESIAN_POINT('',(-1.825,-7.,5.77));
#15848=CARTESIAN_POINT('Origin',(-1.55,-7.,5.77));
#15849=CARTESIAN_POINT('',(-1.7,-7.,5.77));
#15850=CARTESIAN_POINT('Origin',(-1.55,-7.,5.77));
#15851=CARTESIAN_POINT('Origin',(-1.55,-7.,5.77));
#15852=CARTESIAN_POINT('',(-1.825,-6.7,5.77));
#15853=CARTESIAN_POINT('Origin',(-1.55,-6.7,5.77));
#15854=CARTESIAN_POINT('',(-1.825,-7.,5.77));
#15855=CARTESIAN_POINT('Origin',(-1.55,-6.7,5.77));
#15856=CARTESIAN_POINT('Origin',(-1.55,-8.,5.77));
#15857=CARTESIAN_POINT('',(-1.7,-8.,5.77));
#15858=CARTESIAN_POINT('',(-1.7,-8.,5.77));
#15859=CARTESIAN_POINT('Origin',(-1.55,-8.,5.77));
#15860=CARTESIAN_POINT('Origin',(-1.55,-8.,5.77));
#15861=CARTESIAN_POINT('',(0.,0.,0.));
#15862=CARTESIAN_POINT('Origin',(1.40566243270259,-6.9,2.67));
#15863=CARTESIAN_POINT('',(1.4778312163513,-6.7,2.795));
#15864=CARTESIAN_POINT('',(1.40566243270259,-6.7,2.67));
#15865=CARTESIAN_POINT('',(1.42370462861477,-6.7,2.70125));
#15866=CARTESIAN_POINT('',(1.4778312163513,-6.9,2.795));
#15867=CARTESIAN_POINT('',(1.4778312163513,-6.9,2.795));
#15868=CARTESIAN_POINT('',(1.40566243270259,-6.9,2.67));
#15869=CARTESIAN_POINT('',(1.4778312163513,-6.9,2.795));
#15870=CARTESIAN_POINT('',(1.40566243270259,-6.9,2.67));
#15871=CARTESIAN_POINT('Origin',(1.4778312163513,-6.9,2.545));
#15872=CARTESIAN_POINT('',(1.4778312163513,-6.7,2.545));
#15873=CARTESIAN_POINT('',(1.45978902043912,-6.7,2.57625));
#15874=CARTESIAN_POINT('',(1.4778312163513,-6.9,2.545));
#15875=CARTESIAN_POINT('',(1.40566243270259,-6.9,2.67));
#15876=CARTESIAN_POINT('',(1.4778312163513,-6.9,2.545));
#15877=CARTESIAN_POINT('Origin',(1.6221687836487,-6.9,2.545));
#15878=CARTESIAN_POINT('',(1.6221687836487,-6.7,2.545));
#15879=CARTESIAN_POINT('',(1.58608439182435,-6.7,2.545));
#15880=CARTESIAN_POINT('',(1.6221687836487,-6.9,2.545));
#15881=CARTESIAN_POINT('',(1.4778312163513,-6.9,2.545));
#15882=CARTESIAN_POINT('',(1.6221687836487,-6.9,2.545));
#15883=CARTESIAN_POINT('Origin',(1.69433756729741,-6.9,2.67));
#15884=CARTESIAN_POINT('',(1.69433756729741,-6.7,2.67));
#15885=CARTESIAN_POINT('',(1.67629537138523,-6.7,2.63875));
#15886=CARTESIAN_POINT('',(1.69433756729741,-6.9,2.67));
#15887=CARTESIAN_POINT('',(1.6221687836487,-6.9,2.545));
#15888=CARTESIAN_POINT('',(1.69433756729741,-6.9,2.67));
#15889=CARTESIAN_POINT('Origin',(1.6221687836487,-6.9,2.795));
#15890=CARTESIAN_POINT('',(1.6221687836487,-6.7,2.795));
#15891=CARTESIAN_POINT('',(1.64021097956088,-6.7,2.76375));
#15892=CARTESIAN_POINT('',(1.6221687836487,-6.9,2.795));
#15893=CARTESIAN_POINT('',(1.69433756729741,-6.9,2.67));
#15894=CARTESIAN_POINT('',(1.6221687836487,-6.9,2.795));
#15895=CARTESIAN_POINT('Origin',(1.4778312163513,-6.9,2.795));
#15896=CARTESIAN_POINT('',(1.51391560817565,-6.7,2.795));
#15897=CARTESIAN_POINT('',(1.6221687836487,-6.9,2.795));
#15898=CARTESIAN_POINT('Origin',(1.55,-6.9,2.67));
#15899=CARTESIAN_POINT('Origin',(1.55,-7.,2.67));
#15900=CARTESIAN_POINT('',(1.275,-7.,2.67));
#15901=CARTESIAN_POINT('Origin',(1.55,-7.,2.67));
#15902=CARTESIAN_POINT('',(1.4,-7.,2.67));
#15903=CARTESIAN_POINT('Origin',(1.55,-7.,2.67));
#15904=CARTESIAN_POINT('Origin',(1.55,-7.,2.67));
#15905=CARTESIAN_POINT('',(1.275,-6.7,2.67));
#15906=CARTESIAN_POINT('Origin',(1.55,-6.7,2.67));
#15907=CARTESIAN_POINT('',(1.275,-7.,2.67));
#15908=CARTESIAN_POINT('Origin',(1.55,-6.7,2.67));
#15909=CARTESIAN_POINT('Origin',(1.55,-8.,2.67));
#15910=CARTESIAN_POINT('',(1.4,-8.,2.67));
#15911=CARTESIAN_POINT('',(1.4,-8.,2.67));
#15912=CARTESIAN_POINT('Origin',(1.55,-8.,2.67));
#15913=CARTESIAN_POINT('Origin',(1.55,-8.,2.67));
#15914=CARTESIAN_POINT('',(0.,0.,0.));
#15915=CARTESIAN_POINT('Origin',(1.40566243270259,-6.9,5.77));
#15916=CARTESIAN_POINT('',(1.4778312163513,-6.7,5.895));
#15917=CARTESIAN_POINT('',(1.40566243270259,-6.7,5.77));
#15918=CARTESIAN_POINT('',(1.42370462861477,-6.7,5.80125));
#15919=CARTESIAN_POINT('',(1.4778312163513,-6.9,5.895));
#15920=CARTESIAN_POINT('',(1.4778312163513,-6.9,5.895));
#15921=CARTESIAN_POINT('',(1.40566243270259,-6.9,5.77));
#15922=CARTESIAN_POINT('',(1.4778312163513,-6.9,5.895));
#15923=CARTESIAN_POINT('',(1.40566243270259,-6.9,5.77));
#15924=CARTESIAN_POINT('Origin',(1.4778312163513,-6.9,5.645));
#15925=CARTESIAN_POINT('',(1.4778312163513,-6.7,5.645));
#15926=CARTESIAN_POINT('',(1.45978902043912,-6.7,5.67625));
#15927=CARTESIAN_POINT('',(1.4778312163513,-6.9,5.645));
#15928=CARTESIAN_POINT('',(1.40566243270259,-6.9,5.77));
#15929=CARTESIAN_POINT('',(1.4778312163513,-6.9,5.645));
#15930=CARTESIAN_POINT('Origin',(1.6221687836487,-6.9,5.645));
#15931=CARTESIAN_POINT('',(1.6221687836487,-6.7,5.645));
#15932=CARTESIAN_POINT('',(1.58608439182435,-6.7,5.645));
#15933=CARTESIAN_POINT('',(1.6221687836487,-6.9,5.645));
#15934=CARTESIAN_POINT('',(1.4778312163513,-6.9,5.645));
#15935=CARTESIAN_POINT('',(1.6221687836487,-6.9,5.645));
#15936=CARTESIAN_POINT('Origin',(1.69433756729741,-6.9,5.77));
#15937=CARTESIAN_POINT('',(1.69433756729741,-6.7,5.77));
#15938=CARTESIAN_POINT('',(1.67629537138523,-6.7,5.73875));
#15939=CARTESIAN_POINT('',(1.69433756729741,-6.9,5.77));
#15940=CARTESIAN_POINT('',(1.6221687836487,-6.9,5.645));
#15941=CARTESIAN_POINT('',(1.69433756729741,-6.9,5.77));
#15942=CARTESIAN_POINT('Origin',(1.6221687836487,-6.9,5.895));
#15943=CARTESIAN_POINT('',(1.6221687836487,-6.7,5.895));
#15944=CARTESIAN_POINT('',(1.64021097956088,-6.7,5.86375));
#15945=CARTESIAN_POINT('',(1.6221687836487,-6.9,5.895));
#15946=CARTESIAN_POINT('',(1.69433756729741,-6.9,5.77));
#15947=CARTESIAN_POINT('',(1.6221687836487,-6.9,5.895));
#15948=CARTESIAN_POINT('Origin',(1.4778312163513,-6.9,5.895));
#15949=CARTESIAN_POINT('',(1.51391560817565,-6.7,5.895));
#15950=CARTESIAN_POINT('',(1.6221687836487,-6.9,5.895));
#15951=CARTESIAN_POINT('Origin',(1.55,-6.9,5.77));
#15952=CARTESIAN_POINT('Origin',(1.55,-7.,5.77));
#15953=CARTESIAN_POINT('',(1.275,-7.,5.77));
#15954=CARTESIAN_POINT('Origin',(1.55,-7.,5.77));
#15955=CARTESIAN_POINT('',(1.4,-7.,5.77));
#15956=CARTESIAN_POINT('Origin',(1.55,-7.,5.77));
#15957=CARTESIAN_POINT('Origin',(1.55,-7.,5.77));
#15958=CARTESIAN_POINT('',(1.275,-6.7,5.77));
#15959=CARTESIAN_POINT('Origin',(1.55,-6.7,5.77));
#15960=CARTESIAN_POINT('',(1.275,-7.,5.77));
#15961=CARTESIAN_POINT('Origin',(1.55,-6.7,5.77));
#15962=CARTESIAN_POINT('Origin',(1.55,-8.,5.77));
#15963=CARTESIAN_POINT('',(1.4,-8.,5.77));
#15964=CARTESIAN_POINT('',(1.4,-8.,5.77));
#15965=CARTESIAN_POINT('Origin',(1.55,-8.,5.77));
#15966=CARTESIAN_POINT('Origin',(1.55,-8.,5.77));
#15967=CARTESIAN_POINT('',(0.,0.,0.));
#15968=CARTESIAN_POINT('',(0.,0.,0.));
#15969=CARTESIAN_POINT('Origin',(0.,1.85,0.));
#15970=CARTESIAN_POINT('',(-0.943451111610983,1.85,-1.82));
#15971=CARTESIAN_POINT('',(0.943451111610983,1.85,-1.82));
#15972=CARTESIAN_POINT('',(0.,1.85,-1.82));
#15973=CARTESIAN_POINT('Origin',(0.,1.85,0.));
#15974=CARTESIAN_POINT('Origin',(0.,0.,0.));
#15975=CARTESIAN_POINT('',(-0.943451111610983,-1.85,-1.82));
#15976=CARTESIAN_POINT('',(-0.943451111610983,-1.65,-1.82));
#15977=CARTESIAN_POINT('',(-0.943451111610983,0.,-1.82));
#15978=CARTESIAN_POINT('',(0.943451111610983,-1.85,-1.82));
#15979=CARTESIAN_POINT('Origin',(0.,-1.85,0.));
#15980=CARTESIAN_POINT('',(0.943451111610983,-1.65,-1.82));
#15981=CARTESIAN_POINT('',(0.943451111610983,0.,-1.82));
#15982=CARTESIAN_POINT('',(-2.05,-1.65,2.51052593825207E-16));
#15983=CARTESIAN_POINT('Origin',(0.,-1.65,0.));
#15984=CARTESIAN_POINT('',(-2.05,-1.14891252930761,-2.51052593825207E-16));
#15985=CARTESIAN_POINT('',(-2.05,0.,2.51052593825207E-16));
#15986=CARTESIAN_POINT('Origin',(0.,-1.14891252930761,0.));
#15987=CARTESIAN_POINT('Origin',(0.,-1.65,0.));
#15988=CARTESIAN_POINT('Origin',(0.,0.,0.));
#15989=CARTESIAN_POINT('',(-2.05,1.14891252930761,2.51052593825207E-16));
#15990=CARTESIAN_POINT('Origin',(0.,1.14891252930761,0.));
#15991=CARTESIAN_POINT('',(-2.05,1.65,2.51052593825207E-16));
#15992=CARTESIAN_POINT('',(-2.05,0.,2.51052593825207E-16));
#15993=CARTESIAN_POINT('',(0.943451111610983,1.65,-1.82));
#15994=CARTESIAN_POINT('Origin',(0.,1.65,0.));
#15995=CARTESIAN_POINT('',(0.943451111610983,0.,-1.82));
#15996=CARTESIAN_POINT('',(-0.943451111610983,1.65,-1.82));
#15997=CARTESIAN_POINT('',(-0.943451111610983,0.,-1.82));
#15998=CARTESIAN_POINT('Origin',(0.,1.65,0.));
#15999=CARTESIAN_POINT('Origin',(0.,-1.85,0.));
#16000=CARTESIAN_POINT('',(0.,-1.85,-1.82));
#16001=CARTESIAN_POINT('Origin',(0.,-1.65,0.));
#16002=CARTESIAN_POINT('',(2.12781578149989,-1.65,-1.82));
#16003=CARTESIAN_POINT('',(0.,-1.65,-1.82));
#16004=CARTESIAN_POINT('',(-2.12781578149989,-1.65,-1.82));
#16005=CARTESIAN_POINT('Origin',(0.,-1.65,0.));
#16006=CARTESIAN_POINT('',(0.,-1.65,-1.82));
#16007=CARTESIAN_POINT('Origin',(0.,0.,0.));
#16008=CARTESIAN_POINT('',(-1.43895998899814E-16,-1.76221774462768E-32,
-2.35));
#16009=CARTESIAN_POINT('',(-1.43895998899814E-16,-1.76221774462768E-32,
2.35));
#16010=CARTESIAN_POINT('Origin',(0.,0.,0.));
#16011=CARTESIAN_POINT('Origin',(0.,1.55,-1.335));
#16012=CARTESIAN_POINT('',(-3.75878787878788,1.55,-1.82));
#16013=CARTESIAN_POINT('',(-2.12781578149989,1.55,-1.82));
#16014=CARTESIAN_POINT('',(0.,1.55,-1.82));
#16015=CARTESIAN_POINT('',(-2.51385336103051,1.55,-1.23310229877152));
#16016=CARTESIAN_POINT('',(-1.68,1.55,-0.84));
#16017=CARTESIAN_POINT('Origin',(0.,1.55,0.));
#16018=CARTESIAN_POINT('Origin',(0.,1.55,-1.335));
#16019=CARTESIAN_POINT('',(2.12781578149989,1.55,-1.82));
#16020=CARTESIAN_POINT('',(3.75878787878788,1.55,-1.82));
#16021=CARTESIAN_POINT('',(0.,1.55,-1.82));
#16022=CARTESIAN_POINT('',(2.51385336103051,1.55,-1.23310229877152));
#16023=CARTESIAN_POINT('Origin',(0.,1.55,0.));
#16024=CARTESIAN_POINT('',(3.78,1.55,-1.83));
#16025=CARTESIAN_POINT('Origin',(0.,-1.55,-1.335));
#16026=CARTESIAN_POINT('',(-2.12781578149989,-1.55,-1.82));
#16027=CARTESIAN_POINT('',(-3.75878787878788,-1.55,-1.82));
#16028=CARTESIAN_POINT('',(0.,-1.55,-1.82));
#16029=CARTESIAN_POINT('',(-2.51385336103051,-1.55,-1.23310229877152));
#16030=CARTESIAN_POINT('Origin',(0.,-1.55,0.));
#16031=CARTESIAN_POINT('',(-1.68,-1.55,-0.84));
#16032=CARTESIAN_POINT('Origin',(-3.78,0.,-1.83));
#16033=CARTESIAN_POINT('',(-3.75878787878788,0.,-1.82));
#16034=CARTESIAN_POINT('',(-2.51385336103051,0.,-1.23310229877152));
#16035=CARTESIAN_POINT('Origin',(0.,-1.55,-1.335));
#16036=CARTESIAN_POINT('',(3.75878787878788,-1.55,-1.82));
#16037=CARTESIAN_POINT('',(2.12781578149989,-1.55,-1.82));
#16038=CARTESIAN_POINT('',(0.,-1.55,-1.82));
#16039=CARTESIAN_POINT('',(2.51385336103051,-1.55,-1.23310229877152));
#16040=CARTESIAN_POINT('',(3.78,-1.55,-1.83));
#16041=CARTESIAN_POINT('Origin',(0.,-1.55,0.));
#16042=CARTESIAN_POINT('Origin',(1.68,0.,-0.84));
#16043=CARTESIAN_POINT('',(3.75878787878788,0.,-1.82));
#16044=CARTESIAN_POINT('',(2.51385336103051,0.,-1.23310229877153));
#16045=CARTESIAN_POINT('Origin',(0.,0.,-1.82));
#16046=CARTESIAN_POINT('',(-6.35,1.9,-1.82));
#16047=CARTESIAN_POINT('',(-6.35,-1.9,-1.82));
#16048=CARTESIAN_POINT('',(-6.35,1.9,-1.82));
#16049=CARTESIAN_POINT('',(6.35,-1.9,-1.82));
#16050=CARTESIAN_POINT('',(-6.35,-1.9,-1.82));
#16051=CARTESIAN_POINT('',(6.35,1.9,-1.82));
#16052=CARTESIAN_POINT('',(6.35,-1.9,-1.82));
#16053=CARTESIAN_POINT('',(6.35,1.9,-1.82));
#16054=CARTESIAN_POINT('',(-2.12781578149989,0.,-1.82));
#16055=CARTESIAN_POINT('',(-2.12781578149989,1.65,-1.82));
#16056=CARTESIAN_POINT('',(-2.12781578149989,0.,-1.82));
#16057=CARTESIAN_POINT('',(0.,1.65,-1.82));
#16058=CARTESIAN_POINT('',(2.12781578149989,1.65,-1.82));
#16059=CARTESIAN_POINT('',(0.,1.65,-1.82));
#16060=CARTESIAN_POINT('',(2.12781578149989,0.,-1.82));
#16061=CARTESIAN_POINT('',(2.12781578149989,0.,-1.82));
#16062=CARTESIAN_POINT('',(4.1,7.9602041944578E-17,-1.82));
#16063=CARTESIAN_POINT('Origin',(4.75,0.,-1.82));
#16064=CARTESIAN_POINT('',(-5.4,7.9602041944578E-17,-1.82));
#16065=CARTESIAN_POINT('Origin',(-4.75,0.,-1.82));
#16066=CARTESIAN_POINT('Origin',(0.,0.,0.));
#16067=CARTESIAN_POINT('',(-1.22049170419139,-1.4,-2.52));
#16068=CARTESIAN_POINT('',(1.22049170419139,-1.4,-2.52));
#16069=CARTESIAN_POINT('Origin',(0.,-1.4,0.));
#16070=CARTESIAN_POINT('',(-1.22049170419139,1.4,-2.52));
#16071=CARTESIAN_POINT('',(-1.22049170419139,0.,-2.52));
#16072=CARTESIAN_POINT('',(1.22049170419139,1.4,-2.52));
#16073=CARTESIAN_POINT('Origin',(0.,1.4,0.));
#16074=CARTESIAN_POINT('',(1.22049170419139,0.,-2.52));
#16075=CARTESIAN_POINT('Origin',(0.,0.,0.));
#16076=CARTESIAN_POINT('Origin',(0.,1.65,0.));
#16077=CARTESIAN_POINT('Origin',(0.,1.65,0.));
#16078=CARTESIAN_POINT('Origin',(3.35,1.4,-3.02));
#16079=CARTESIAN_POINT('',(-3.35,1.4,-2.52));
#16080=CARTESIAN_POINT('',(3.35,1.4,-2.52));
#16081=CARTESIAN_POINT('',(-3.35,1.4,-3.02));
#16082=CARTESIAN_POINT('',(-3.35,1.4,-3.02));
#16083=CARTESIAN_POINT('',(3.35,1.4,-3.02));
#16084=CARTESIAN_POINT('',(1.675,1.4,-3.02));
#16085=CARTESIAN_POINT('',(3.35,1.4,-2.52));
#16086=CARTESIAN_POINT('',(3.35,1.4,-3.02));
#16087=CARTESIAN_POINT('',(3.35,1.4,-2.52));
#16088=CARTESIAN_POINT('Origin',(0.,0.,-2.52));
#16089=CARTESIAN_POINT('',(-3.35,-1.4,-2.52));
#16090=CARTESIAN_POINT('',(-3.35,-1.4,-2.52));
#16091=CARTESIAN_POINT('',(-3.35,1.4,-2.52));
#16092=CARTESIAN_POINT('Origin',(3.35,-1.4,-3.02));
#16093=CARTESIAN_POINT('',(3.35,-1.4,-3.02));
#16094=CARTESIAN_POINT('',(3.35,-0.7,-3.02));
#16095=CARTESIAN_POINT('',(3.35,-1.4,-2.52));
#16096=CARTESIAN_POINT('',(3.35,-1.4,-3.02));
#16097=CARTESIAN_POINT('',(3.35,-1.4,-2.52));
#16098=CARTESIAN_POINT('Origin',(-3.35,-1.4,-3.02));
#16099=CARTESIAN_POINT('',(-3.35,-1.4,-2.52));
#16100=CARTESIAN_POINT('',(-3.35,-1.4,-3.02));
#16101=CARTESIAN_POINT('',(-1.675,-1.4,-3.02));
#16102=CARTESIAN_POINT('',(-3.35,-1.4,-3.02));
#16103=CARTESIAN_POINT('Origin',(-3.35,1.4,-3.02));
#16104=CARTESIAN_POINT('',(-3.35,0.7,-3.02));
#16105=CARTESIAN_POINT('Origin',(0.,0.,-2.52));
#16106=CARTESIAN_POINT('Origin',(-4.75,0.,-3.02));
#16107=CARTESIAN_POINT('',(-5.4,-7.9602041944578E-17,-3.02));
#16108=CARTESIAN_POINT('Origin',(-4.75,0.,-3.02));
#16109=CARTESIAN_POINT('',(-5.4,-7.9602041944578E-17,-3.02));
#16110=CARTESIAN_POINT('Origin',(4.75,0.,-3.02));
#16111=CARTESIAN_POINT('',(4.1,-7.9602041944578E-17,-3.02));
#16112=CARTESIAN_POINT('Origin',(4.75,0.,-3.02));
#16113=CARTESIAN_POINT('',(4.1,-7.9602041944578E-17,-3.02));
#16114=CARTESIAN_POINT('Origin',(6.35,1.9,-3.02));
#16115=CARTESIAN_POINT('',(6.35,1.9,-3.02));
#16116=CARTESIAN_POINT('',(-6.35,1.9,-3.02));
#16117=CARTESIAN_POINT('',(6.35,1.9,-3.02));
#16118=CARTESIAN_POINT('',(-6.35,1.9,-3.02));
#16119=CARTESIAN_POINT('',(6.35,1.9,-3.02));
#16120=CARTESIAN_POINT('Origin',(6.35,-1.9,-3.02));
#16121=CARTESIAN_POINT('',(6.35,-1.9,-3.02));
#16122=CARTESIAN_POINT('',(6.35,-1.9,-3.02));
#16123=CARTESIAN_POINT('',(6.35,-1.9,-3.02));
#16124=CARTESIAN_POINT('Origin',(-6.35,-1.9,-3.02));
#16125=CARTESIAN_POINT('',(-6.35,-1.9,-3.02));
#16126=CARTESIAN_POINT('',(-6.35,-1.9,-3.02));
#16127=CARTESIAN_POINT('',(-6.35,-1.9,-3.02));
#16128=CARTESIAN_POINT('Origin',(-6.35,1.9,-3.02));
#16129=CARTESIAN_POINT('',(-6.35,1.9,-3.02));
#16130=CARTESIAN_POINT('Origin',(0.,0.,-3.02));
#16131=CARTESIAN_POINT('',(0.,0.,0.));
#16132=CARTESIAN_POINT('Origin',(0.,0.,0.));
#16133=CARTESIAN_POINT('',(-1.8,-0.85,-2.20436423846524E-16));
#16134=CARTESIAN_POINT('Origin',(0.,-0.85,0.));
#16135=CARTESIAN_POINT('',(-1.8,0.85,-2.20436423846524E-16));
#16136=CARTESIAN_POINT('',(-1.8,0.,-2.20436423846524E-16));
#16137=CARTESIAN_POINT('Origin',(0.,0.85,0.));
#16138=CARTESIAN_POINT('Origin',(2.19089023002066,0.85,0.));
#16139=CARTESIAN_POINT('',(2.19089023002066,0.85,0.));
#16140=CARTESIAN_POINT('Origin',(0.,0.85,0.));
#16141=CARTESIAN_POINT('Origin',(3.99680288865056E-15,0.,0.));
#16142=CARTESIAN_POINT('',(3.85290688975075E-15,-1.76221774462768E-32,2.35));
#16143=CARTESIAN_POINT('',(3.85290688975075E-15,-1.76221774462768E-32,-2.35));
#16144=CARTESIAN_POINT('Origin',(3.99680288865056E-15,0.,0.));
#16145=CARTESIAN_POINT('',(2.19089023002066,-0.85,0.));
#16146=CARTESIAN_POINT('Origin',(0.,-0.85,0.));
#16147=CARTESIAN_POINT('Origin',(1.8,-0.85,0.));
#16148=CARTESIAN_POINT('Origin',(0.,1.55,0.));
#16149=CARTESIAN_POINT('',(1.42894191624432,1.8,0.825000000000001));
#16150=CARTESIAN_POINT('',(1.53744468918255,1.55,0.598968970568896));
#16151=CARTESIAN_POINT('Ctrl Pts',(1.42894191624432,1.8,0.825000000000001));
#16152=CARTESIAN_POINT('Ctrl Pts',(1.44466308895875,1.8,0.797770130104052));
#16153=CARTESIAN_POINT('Ctrl Pts',(1.46055812562105,1.79370633789704,0.768258557763732));
#16154=CARTESIAN_POINT('Ctrl Pts',(1.48824888379079,1.76817777258318,0.713138492740816));
#16155=CARTESIAN_POINT('Ctrl Pts',(1.50008999307766,1.74894552961493,0.687551581002689));
#16156=CARTESIAN_POINT('Ctrl Pts',(1.51812136280714,1.70460745840382,0.646764802471699));
#16157=CARTESIAN_POINT('Ctrl Pts',(1.52552758004446,1.67652816181843,0.628833667319578));
#16158=CARTESIAN_POINT('Ctrl Pts',(1.53516661651472,1.61494799959182,0.604921184808251));
#16159=CARTESIAN_POINT('Ctrl Pts',(1.53744468918255,1.58144291640553,0.598968970568896));
#16160=CARTESIAN_POINT('Ctrl Pts',(1.53744468918255,1.55,0.598968970568896));
#16161=CARTESIAN_POINT('',(1.42894191624432,1.3,0.825000000000001));
#16162=CARTESIAN_POINT('Ctrl Pts',(1.42894191624432,1.3,0.825000000000001));
#16163=CARTESIAN_POINT('Ctrl Pts',(1.4132207435299,1.3,0.852229869895949));
#16164=CARTESIAN_POINT('Ctrl Pts',(1.39561049050871,1.30629366210296,0.880751161609749));
#16165=CARTESIAN_POINT('Ctrl Pts',(1.36172049302549,1.33182222741682,0.932292094146256));
#16166=CARTESIAN_POINT('Ctrl Pts',(1.34548213209931,1.35105447038507,0.955340251466734));
#16167=CARTESIAN_POINT('Ctrl Pts',(1.31917543061769,1.39539254159618,0.99134926498299));
#16168=CARTESIAN_POINT('Ctrl Pts',(1.30734972067592,1.42347183818157,1.00672880483252));
#16169=CARTESIAN_POINT('Ctrl Pts',(1.29146042158868,1.48505200040818,1.02703269653942));
#16170=CARTESIAN_POINT('Ctrl Pts',(1.28744468918255,1.51855708359447,1.03198167246111));
#16171=CARTESIAN_POINT('Ctrl Pts',(1.28744468918255,1.58144291640553,1.03198167246111));
#16172=CARTESIAN_POINT('Ctrl Pts',(1.29146042158868,1.61494799959182,1.02703269653942));
#16173=CARTESIAN_POINT('Ctrl Pts',(1.30734972067592,1.67652816181843,1.00672880483252));
#16174=CARTESIAN_POINT('Ctrl Pts',(1.31917543061769,1.70460745840382,0.991349264982991));
#16175=CARTESIAN_POINT('Ctrl Pts',(1.34548213209931,1.74894552961493,0.955340251466735));
#16176=CARTESIAN_POINT('Ctrl Pts',(1.36172049302549,1.76817777258318,0.932292094146256));
#16177=CARTESIAN_POINT('Ctrl Pts',(1.39561049050871,1.79370633789704,0.880751161609749));
#16178=CARTESIAN_POINT('Ctrl Pts',(1.4132207435299,1.8,0.85222986989595));
#16179=CARTESIAN_POINT('Ctrl Pts',(1.42894191624432,1.8,0.825000000000001));
#16180=CARTESIAN_POINT('Ctrl Pts',(1.53744468918255,1.55,0.598968970568896));
#16181=CARTESIAN_POINT('Ctrl Pts',(1.53744468918255,1.51855708359447,0.598968970568896));
#16182=CARTESIAN_POINT('Ctrl Pts',(1.53516661651472,1.48505200040818,0.60492118480825));
#16183=CARTESIAN_POINT('Ctrl Pts',(1.52552758004446,1.42347183818157,0.628833667319578));
#16184=CARTESIAN_POINT('Ctrl Pts',(1.51812136280714,1.39539254159618,0.646764802471699));
#16185=CARTESIAN_POINT('Ctrl Pts',(1.50008999307766,1.35105447038507,0.687551581002689));
#16186=CARTESIAN_POINT('Ctrl Pts',(1.48824888379079,1.33182222741682,0.713138492740816));
#16187=CARTESIAN_POINT('Ctrl Pts',(1.46055812562105,1.30629366210296,0.768258557763732));
#16188=CARTESIAN_POINT('Ctrl Pts',(1.44466308895875,1.3,0.797770130104052));
#16189=CARTESIAN_POINT('Ctrl Pts',(1.42894191624432,1.3,0.825000000000001));
#16190=CARTESIAN_POINT('',(0.59736109069228,1.55,0.0562114519197835));
#16191=CARTESIAN_POINT('',(0.125,1.55,-0.21650635094611));
#16192=CARTESIAN_POINT('Ctrl Pts',(0.59736109069228,1.55,0.0562114519197835));
#16193=CARTESIAN_POINT('Ctrl Pts',(0.59736109069228,1.58183602855499,0.0562114519197835));
#16194=CARTESIAN_POINT('Ctrl Pts',(0.596809586309859,1.61548166177648,0.0633319361811907));
#16195=CARTESIAN_POINT('Ctrl Pts',(0.593243052195919,1.67693412158597,0.0908585874761106));
#16196=CARTESIAN_POINT('Ctrl Pts',(0.590063593315144,1.70478184753241,0.111151766652641));
#16197=CARTESIAN_POINT('Ctrl Pts',(0.579820497891285,1.74874496453875,0.15600214762839));
#16198=CARTESIAN_POINT('Ctrl Pts',(0.572042315803119,1.76792916820474,0.183678633836535));
#16199=CARTESIAN_POINT('Ctrl Pts',(0.549947124580676,1.79356669468566,0.241926459727039));
#16200=CARTESIAN_POINT('Ctrl Pts',(0.53551402125728,1.8,0.27246250701687));
#16201=CARTESIAN_POINT('Ctrl Pts',(0.503716463284046,1.8,0.32753749298313));
#16202=CARTESIAN_POINT('Ctrl Pts',(0.484488022261586,1.79356669468566,0.355304950761552));
#16203=CARTESIAN_POINT('Ctrl Pts',(0.445091520936419,1.76792916820474,0.403563860606914));
#16204=CARTESIAN_POINT('Ctrl Pts',(0.425012071836758,1.74874496453875,0.4241382069946));
#16205=CARTESIAN_POINT('Ctrl Pts',(0.391292050254278,1.70478184753241,0.455434178332924));
#16206=CARTESIAN_POINT('Ctrl Pts',(0.375307371004241,1.67693412158597,0.468334260082228));
#16207=CARTESIAN_POINT('Ctrl Pts',(0.353251858758695,1.61548166177647,0.485186294875824));
#16208=CARTESIAN_POINT('Ctrl Pts',(0.347361090692279,1.58183602855499,0.489224153812003));
#16209=CARTESIAN_POINT('Ctrl Pts',(0.347361090692279,1.51816397144501,0.489224153812003));
#16210=CARTESIAN_POINT('Ctrl Pts',(0.353251858758695,1.48451833822352,0.485186294875824));
#16211=CARTESIAN_POINT('Ctrl Pts',(0.375307371004241,1.42306587841403,0.468334260082228));
#16212=CARTESIAN_POINT('Ctrl Pts',(0.391292050254278,1.39521815246759,0.455434178332924));
#16213=CARTESIAN_POINT('Ctrl Pts',(0.425012071836758,1.35125503546125,0.4241382069946));
#16214=CARTESIAN_POINT('Ctrl Pts',(0.445091520936418,1.33207083179526,0.403563860606914));
#16215=CARTESIAN_POINT('Ctrl Pts',(0.484488022261586,1.30643330531434,0.355304950761552));
#16216=CARTESIAN_POINT('Ctrl Pts',(0.503716463284046,1.3,0.32753749298313));
#16217=CARTESIAN_POINT('Ctrl Pts',(0.53551402125728,1.3,0.27246250701687));
#16218=CARTESIAN_POINT('Ctrl Pts',(0.549947124580676,1.30643330531434,0.241926459727039));
#16219=CARTESIAN_POINT('Ctrl Pts',(0.572042315803119,1.33207083179526,0.183678633836535));
#16220=CARTESIAN_POINT('Ctrl Pts',(0.579820497891285,1.35125503546125,0.15600214762839));
#16221=CARTESIAN_POINT('Ctrl Pts',(0.590063593315144,1.39521815246759,0.111151766652641));
#16222=CARTESIAN_POINT('Ctrl Pts',(0.593243052195919,1.42306587841403,0.0908585874761105));
#16223=CARTESIAN_POINT('Ctrl Pts',(0.596809586309859,1.48451833822352,0.0633319361811906));
#16224=CARTESIAN_POINT('Ctrl Pts',(0.59736109069228,1.51816397144501,0.0562114519197835));
#16225=CARTESIAN_POINT('Ctrl Pts',(0.59736109069228,1.55,0.0562114519197835));
#16226=CARTESIAN_POINT('Origin',(0.,1.55,0.));
#16227=CARTESIAN_POINT('',(-0.347361090692279,1.55,-0.489224153812003));
#16228=CARTESIAN_POINT('Ctrl Pts',(-0.347361090692279,1.55,-0.489224153812003));
#16229=CARTESIAN_POINT('Ctrl Pts',(-0.347361090692279,1.51816397144501,
-0.489224153812003));
#16230=CARTESIAN_POINT('Ctrl Pts',(-0.353251858758695,1.48451833822352,
-0.485186294875824));
#16231=CARTESIAN_POINT('Ctrl Pts',(-0.375307371004241,1.42306587841403,
-0.468334260082228));
#16232=CARTESIAN_POINT('Ctrl Pts',(-0.391292050254278,1.39521815246759,
-0.455434178332924));
#16233=CARTESIAN_POINT('Ctrl Pts',(-0.425012071836758,1.35125503546125,
-0.4241382069946));
#16234=CARTESIAN_POINT('Ctrl Pts',(-0.445091520936419,1.33207083179526,
-0.403563860606914));
#16235=CARTESIAN_POINT('Ctrl Pts',(-0.484488022261586,1.30643330531434,
-0.355304950761552));
#16236=CARTESIAN_POINT('Ctrl Pts',(-0.503716463284046,1.3,-0.32753749298313));
#16237=CARTESIAN_POINT('Ctrl Pts',(-0.53551402125728,1.3,-0.27246250701687));
#16238=CARTESIAN_POINT('Ctrl Pts',(-0.549947124580676,1.30643330531434,
-0.241926459727039));
#16239=CARTESIAN_POINT('Ctrl Pts',(-0.572042315803119,1.33207083179526,
-0.183678633836535));
#16240=CARTESIAN_POINT('Ctrl Pts',(-0.579820497891285,1.35125503546125,
-0.15600214762839));
#16241=CARTESIAN_POINT('Ctrl Pts',(-0.590063593315144,1.39521815246759,
-0.111151766652641));
#16242=CARTESIAN_POINT('Ctrl Pts',(-0.593243052195918,1.42306587841403,
-0.0908585874761106));
#16243=CARTESIAN_POINT('Ctrl Pts',(-0.596809586309859,1.48451833822352,
-0.0633319361811906));
#16244=CARTESIAN_POINT('Ctrl Pts',(-0.597361090692279,1.51816397144501,
-0.0562114519197835));
#16245=CARTESIAN_POINT('Ctrl Pts',(-0.597361090692279,1.58183602855499,
-0.0562114519197835));
#16246=CARTESIAN_POINT('Ctrl Pts',(-0.596809586309859,1.61548166177647,
-0.0633319361811905));
#16247=CARTESIAN_POINT('Ctrl Pts',(-0.593243052195918,1.67693412158597,
-0.0908585874761104));
#16248=CARTESIAN_POINT('Ctrl Pts',(-0.590063593315144,1.70478184753241,
-0.111151766652641));
#16249=CARTESIAN_POINT('Ctrl Pts',(-0.579820497891285,1.74874496453875,
-0.15600214762839));
#16250=CARTESIAN_POINT('Ctrl Pts',(-0.572042315803118,1.76792916820474,
-0.183678633836535));
#16251=CARTESIAN_POINT('Ctrl Pts',(-0.549947124580676,1.79356669468566,
-0.241926459727039));
#16252=CARTESIAN_POINT('Ctrl Pts',(-0.53551402125728,1.8,-0.27246250701687));
#16253=CARTESIAN_POINT('Ctrl Pts',(-0.503716463284046,1.8,-0.32753749298313));
#16254=CARTESIAN_POINT('Ctrl Pts',(-0.484488022261586,1.79356669468566,
-0.355304950761552));
#16255=CARTESIAN_POINT('Ctrl Pts',(-0.445091520936419,1.76792916820474,
-0.403563860606914));
#16256=CARTESIAN_POINT('Ctrl Pts',(-0.425012071836758,1.74874496453875,
-0.4241382069946));
#16257=CARTESIAN_POINT('Ctrl Pts',(-0.391292050254278,1.70478184753241,
-0.455434178332924));
#16258=CARTESIAN_POINT('Ctrl Pts',(-0.375307371004241,1.67693412158597,
-0.468334260082228));
#16259=CARTESIAN_POINT('Ctrl Pts',(-0.353251858758695,1.61548166177648,
-0.485186294875824));
#16260=CARTESIAN_POINT('Ctrl Pts',(-0.347361090692279,1.58183602855499,
-0.489224153812003));
#16261=CARTESIAN_POINT('Ctrl Pts',(-0.347361090692279,1.55,-0.489224153812003));
#16262=CARTESIAN_POINT('',(-1.28744468918255,1.55,-1.03198167246111));
#16263=CARTESIAN_POINT('',(0.125,1.55,-0.21650635094611));
#16264=CARTESIAN_POINT('',(-1.42894191624432,1.3,-0.825000000000001));
#16265=CARTESIAN_POINT('Ctrl Pts',(-1.42894191624432,1.3,-0.825000000000001));
#16266=CARTESIAN_POINT('Ctrl Pts',(-1.4132207435299,1.3,-0.852229869895949));
#16267=CARTESIAN_POINT('Ctrl Pts',(-1.39561049050871,1.30629366210296,-0.880751161609749));
#16268=CARTESIAN_POINT('Ctrl Pts',(-1.36172049302549,1.33182222741682,-0.932292094146256));
#16269=CARTESIAN_POINT('Ctrl Pts',(-1.34548213209931,1.35105447038507,-0.955340251466735));
#16270=CARTESIAN_POINT('Ctrl Pts',(-1.31917543061769,1.39539254159618,-0.991349264982991));
#16271=CARTESIAN_POINT('Ctrl Pts',(-1.30734972067592,1.42347183818157,-1.00672880483252));
#16272=CARTESIAN_POINT('Ctrl Pts',(-1.29146042158868,1.48505200040818,-1.02703269653942));
#16273=CARTESIAN_POINT('Ctrl Pts',(-1.28744468918255,1.51855708359447,-1.03198167246111));
#16274=CARTESIAN_POINT('Ctrl Pts',(-1.28744468918255,1.55,-1.03198167246111));
#16275=CARTESIAN_POINT('',(-1.42894191624432,1.8,-0.825000000000001));
#16276=CARTESIAN_POINT('Ctrl Pts',(-1.42894191624432,1.8,-0.825000000000001));
#16277=CARTESIAN_POINT('Ctrl Pts',(-1.44466308895875,1.8,-0.797770130104052));
#16278=CARTESIAN_POINT('Ctrl Pts',(-1.46055812562105,1.79370633789704,-0.768258557763732));
#16279=CARTESIAN_POINT('Ctrl Pts',(-1.48824888379079,1.76817777258318,-0.713138492740816));
#16280=CARTESIAN_POINT('Ctrl Pts',(-1.50008999307766,1.74894552961493,-0.687551581002689));
#16281=CARTESIAN_POINT('Ctrl Pts',(-1.51812136280714,1.70460745840382,-0.646764802471699));
#16282=CARTESIAN_POINT('Ctrl Pts',(-1.52552758004446,1.67652816181843,-0.628833667319578));
#16283=CARTESIAN_POINT('Ctrl Pts',(-1.53516661651472,1.61494799959182,-0.60492118480825));
#16284=CARTESIAN_POINT('Ctrl Pts',(-1.53744468918255,1.58144291640553,-0.598968970568896));
#16285=CARTESIAN_POINT('Ctrl Pts',(-1.53744468918255,1.51855708359447,-0.598968970568896));
#16286=CARTESIAN_POINT('Ctrl Pts',(-1.53516661651472,1.48505200040818,-0.60492118480825));
#16287=CARTESIAN_POINT('Ctrl Pts',(-1.52552758004446,1.42347183818157,-0.628833667319578));
#16288=CARTESIAN_POINT('Ctrl Pts',(-1.51812136280714,1.39539254159618,-0.646764802471699));
#16289=CARTESIAN_POINT('Ctrl Pts',(-1.50008999307766,1.35105447038507,-0.687551581002689));
#16290=CARTESIAN_POINT('Ctrl Pts',(-1.48824888379079,1.33182222741682,-0.713138492740816));
#16291=CARTESIAN_POINT('Ctrl Pts',(-1.46055812562105,1.30629366210296,-0.768258557763732));
#16292=CARTESIAN_POINT('Ctrl Pts',(-1.44466308895875,1.3,-0.797770130104052));
#16293=CARTESIAN_POINT('Ctrl Pts',(-1.42894191624432,1.3,-0.825000000000001));
#16294=CARTESIAN_POINT('Ctrl Pts',(-1.28744468918255,1.55,-1.03198167246111));
#16295=CARTESIAN_POINT('Ctrl Pts',(-1.28744468918255,1.58144291640553,-1.03198167246111));
#16296=CARTESIAN_POINT('Ctrl Pts',(-1.29146042158868,1.61494799959182,-1.02703269653942));
#16297=CARTESIAN_POINT('Ctrl Pts',(-1.30734972067592,1.67652816181843,-1.00672880483252));
#16298=CARTESIAN_POINT('Ctrl Pts',(-1.31917543061769,1.70460745840382,-0.991349264982991));
#16299=CARTESIAN_POINT('Ctrl Pts',(-1.34548213209931,1.74894552961493,-0.955340251466734));
#16300=CARTESIAN_POINT('Ctrl Pts',(-1.36172049302549,1.76817777258318,-0.932292094146256));
#16301=CARTESIAN_POINT('Ctrl Pts',(-1.39561049050871,1.79370633789704,-0.880751161609749));
#16302=CARTESIAN_POINT('Ctrl Pts',(-1.4132207435299,1.8,-0.852229869895949));
#16303=CARTESIAN_POINT('Ctrl Pts',(-1.42894191624432,1.8,-0.825000000000001));
#16304=CARTESIAN_POINT('Origin',(0.,1.55,0.));
#16305=CARTESIAN_POINT('',(-1.65,0.85,-2.02066721859313E-16));
#16306=CARTESIAN_POINT('Origin',(0.,0.85,0.));
#16307=CARTESIAN_POINT('',(-1.65,2.25,-2.02066721859313E-16));
#16308=CARTESIAN_POINT('',(-1.65,1.55,-2.02066721859313E-16));
#16309=CARTESIAN_POINT('Origin',(0.,2.25,0.));
#16310=CARTESIAN_POINT('',(-1.42894191624432,1.3,0.825));
#16311=CARTESIAN_POINT('',(-1.42894191624432,1.8,0.825));
#16312=CARTESIAN_POINT('Ctrl Pts',(-1.42894191624432,1.3,0.825));
#16313=CARTESIAN_POINT('Ctrl Pts',(-1.44466308895875,1.3,0.797770130104051));
#16314=CARTESIAN_POINT('Ctrl Pts',(-1.46055812562105,1.30629366210296,0.768258557763731));
#16315=CARTESIAN_POINT('Ctrl Pts',(-1.48824888379079,1.33182222741682,0.713138492740815));
#16316=CARTESIAN_POINT('Ctrl Pts',(-1.50008999307766,1.35105447038507,0.687551581002688));
#16317=CARTESIAN_POINT('Ctrl Pts',(-1.51812136280714,1.39539254159618,0.646764802471698));
#16318=CARTESIAN_POINT('Ctrl Pts',(-1.52552758004446,1.42347183818157,0.628833667319577));
#16319=CARTESIAN_POINT('Ctrl Pts',(-1.53516661651472,1.48505200040818,0.604921184808249));
#16320=CARTESIAN_POINT('Ctrl Pts',(-1.53744468918255,1.51855708359447,0.598968970568895));
#16321=CARTESIAN_POINT('Ctrl Pts',(-1.53744468918255,1.58144291640553,0.598968970568895));
#16322=CARTESIAN_POINT('Ctrl Pts',(-1.53516661651472,1.61494799959182,0.604921184808249));
#16323=CARTESIAN_POINT('Ctrl Pts',(-1.52552758004446,1.67652816181843,0.628833667319577));
#16324=CARTESIAN_POINT('Ctrl Pts',(-1.51812136280714,1.70460745840382,0.646764802471698));
#16325=CARTESIAN_POINT('Ctrl Pts',(-1.50008999307766,1.74894552961493,0.687551581002688));
#16326=CARTESIAN_POINT('Ctrl Pts',(-1.48824888379079,1.76817777258318,0.713138492740815));
#16327=CARTESIAN_POINT('Ctrl Pts',(-1.46055812562105,1.79370633789704,0.768258557763731));
#16328=CARTESIAN_POINT('Ctrl Pts',(-1.44466308895875,1.8,0.797770130104051));
#16329=CARTESIAN_POINT('Ctrl Pts',(-1.42894191624432,1.8,0.825));
#16330=CARTESIAN_POINT('',(-1.28744468918255,1.55,1.03198167246111));
#16331=CARTESIAN_POINT('Ctrl Pts',(-1.42894191624432,1.8,0.825));
#16332=CARTESIAN_POINT('Ctrl Pts',(-1.4132207435299,1.8,0.852229869895948));
#16333=CARTESIAN_POINT('Ctrl Pts',(-1.39561049050871,1.79370633789704,0.880751161609747));
#16334=CARTESIAN_POINT('Ctrl Pts',(-1.36172049302549,1.76817777258318,0.932292094146255));
#16335=CARTESIAN_POINT('Ctrl Pts',(-1.34548213209931,1.74894552961493,0.955340251466733));
#16336=CARTESIAN_POINT('Ctrl Pts',(-1.31917543061769,1.70460745840382,0.991349264982989));
#16337=CARTESIAN_POINT('Ctrl Pts',(-1.30734972067592,1.67652816181843,1.00672880483252));
#16338=CARTESIAN_POINT('Ctrl Pts',(-1.29146042158868,1.61494799959182,1.02703269653942));
#16339=CARTESIAN_POINT('Ctrl Pts',(-1.28744468918255,1.58144291640553,1.03198167246111));
#16340=CARTESIAN_POINT('Ctrl Pts',(-1.28744468918255,1.55,1.03198167246111));
#16341=CARTESIAN_POINT('Ctrl Pts',(-1.28744468918255,1.55,1.03198167246111));
#16342=CARTESIAN_POINT('Ctrl Pts',(-1.28744468918255,1.51855708359447,1.03198167246111));
#16343=CARTESIAN_POINT('Ctrl Pts',(-1.29146042158868,1.48505200040818,1.02703269653942));
#16344=CARTESIAN_POINT('Ctrl Pts',(-1.30734972067592,1.42347183818157,1.00672880483252));
#16345=CARTESIAN_POINT('Ctrl Pts',(-1.31917543061769,1.39539254159618,0.99134926498299));
#16346=CARTESIAN_POINT('Ctrl Pts',(-1.34548213209931,1.35105447038508,0.955340251466733));
#16347=CARTESIAN_POINT('Ctrl Pts',(-1.36172049302549,1.33182222741682,0.932292094146255));
#16348=CARTESIAN_POINT('Ctrl Pts',(-1.39561049050871,1.30629366210296,0.880751161609748));
#16349=CARTESIAN_POINT('Ctrl Pts',(-1.4132207435299,1.3,0.852229869895949));
#16350=CARTESIAN_POINT('Ctrl Pts',(-1.42894191624432,1.3,0.825));
#16351=CARTESIAN_POINT('',(1.42894191624432,1.8,-0.825));
#16352=CARTESIAN_POINT('',(1.42894191624432,1.3,-0.825));
#16353=CARTESIAN_POINT('Ctrl Pts',(1.42894191624432,1.8,-0.825));
#16354=CARTESIAN_POINT('Ctrl Pts',(1.4132207435299,1.8,-0.852229869895949));
#16355=CARTESIAN_POINT('Ctrl Pts',(1.39561049050871,1.79370633789704,-0.880751161609748));
#16356=CARTESIAN_POINT('Ctrl Pts',(1.36172049302549,1.76817777258318,-0.932292094146255));
#16357=CARTESIAN_POINT('Ctrl Pts',(1.34548213209931,1.74894552961493,-0.955340251466734));
#16358=CARTESIAN_POINT('Ctrl Pts',(1.31917543061769,1.70460745840382,-0.99134926498299));
#16359=CARTESIAN_POINT('Ctrl Pts',(1.30734972067592,1.67652816181843,-1.00672880483252));
#16360=CARTESIAN_POINT('Ctrl Pts',(1.29146042158868,1.61494799959182,-1.02703269653942));
#16361=CARTESIAN_POINT('Ctrl Pts',(1.28744468918255,1.58144291640553,-1.03198167246111));
#16362=CARTESIAN_POINT('Ctrl Pts',(1.28744468918255,1.51855708359447,-1.03198167246111));
#16363=CARTESIAN_POINT('Ctrl Pts',(1.29146042158868,1.48505200040818,-1.02703269653942));
#16364=CARTESIAN_POINT('Ctrl Pts',(1.30734972067592,1.42347183818157,-1.00672880483252));
#16365=CARTESIAN_POINT('Ctrl Pts',(1.31917543061769,1.39539254159618,-0.99134926498299));
#16366=CARTESIAN_POINT('Ctrl Pts',(1.34548213209931,1.35105447038507,-0.955340251466734));
#16367=CARTESIAN_POINT('Ctrl Pts',(1.36172049302549,1.33182222741682,-0.932292094146255));
#16368=CARTESIAN_POINT('Ctrl Pts',(1.39561049050871,1.30629366210296,-0.880751161609748));
#16369=CARTESIAN_POINT('Ctrl Pts',(1.4132207435299,1.3,-0.852229869895948));
#16370=CARTESIAN_POINT('Ctrl Pts',(1.42894191624432,1.3,-0.825));
#16371=CARTESIAN_POINT('',(1.53744468918255,1.55,-0.598968970568895));
#16372=CARTESIAN_POINT('Ctrl Pts',(1.42894191624432,1.3,-0.825));
#16373=CARTESIAN_POINT('Ctrl Pts',(1.44466308895875,1.3,-0.797770130104051));
#16374=CARTESIAN_POINT('Ctrl Pts',(1.46055812562105,1.30629366210296,-0.768258557763731));
#16375=CARTESIAN_POINT('Ctrl Pts',(1.48824888379079,1.33182222741682,-0.713138492740815));
#16376=CARTESIAN_POINT('Ctrl Pts',(1.50008999307766,1.35105447038507,-0.687551581002688));
#16377=CARTESIAN_POINT('Ctrl Pts',(1.51812136280714,1.39539254159618,-0.646764802471698));
#16378=CARTESIAN_POINT('Ctrl Pts',(1.52552758004446,1.42347183818157,-0.628833667319577));
#16379=CARTESIAN_POINT('Ctrl Pts',(1.53516661651472,1.48505200040818,-0.604921184808249));
#16380=CARTESIAN_POINT('Ctrl Pts',(1.53744468918255,1.51855708359447,-0.598968970568895));
#16381=CARTESIAN_POINT('Ctrl Pts',(1.53744468918255,1.55,-0.598968970568895));
#16382=CARTESIAN_POINT('Ctrl Pts',(1.53744468918255,1.55,-0.598968970568895));
#16383=CARTESIAN_POINT('Ctrl Pts',(1.53744468918255,1.58144291640553,-0.598968970568895));
#16384=CARTESIAN_POINT('Ctrl Pts',(1.53516661651472,1.61494799959182,-0.604921184808249));
#16385=CARTESIAN_POINT('Ctrl Pts',(1.52552758004446,1.67652816181843,-0.628833667319577));
#16386=CARTESIAN_POINT('Ctrl Pts',(1.51812136280714,1.70460745840382,-0.646764802471698));
#16387=CARTESIAN_POINT('Ctrl Pts',(1.50008999307766,1.74894552961493,-0.687551581002688));
#16388=CARTESIAN_POINT('Ctrl Pts',(1.48824888379079,1.76817777258318,-0.713138492740815));
#16389=CARTESIAN_POINT('Ctrl Pts',(1.46055812562105,1.79370633789704,-0.768258557763731));
#16390=CARTESIAN_POINT('Ctrl Pts',(1.44466308895875,1.8,-0.797770130104051));
#16391=CARTESIAN_POINT('Ctrl Pts',(1.42894191624432,1.8,-0.825));
#16392=CARTESIAN_POINT('',(0.,1.3,-1.65));
#16393=CARTESIAN_POINT('',(0.,1.8,-1.65));
#16394=CARTESIAN_POINT('Ctrl Pts',(1.38777878078145E-17,1.3,-1.65));
#16395=CARTESIAN_POINT('Ctrl Pts',(0.0314423454288489,1.3,-1.65));
#16396=CARTESIAN_POINT('Ctrl Pts',(0.0649476351123396,1.30629366210296,
-1.64900971937348));
#16397=CARTESIAN_POINT('Ctrl Pts',(0.126528390765307,1.33182222741682,-1.64543058688707));
#16398=CARTESIAN_POINT('Ctrl Pts',(0.154607860978348,1.35105447038507,-1.64289183246942));
#16399=CARTESIAN_POINT('Ctrl Pts',(0.198945932189457,1.39539254159618,-1.63811406745469));
#16400=CARTESIAN_POINT('Ctrl Pts',(0.218177859368546,1.42347183818157,-1.63556247215209));
#16401=CARTESIAN_POINT('Ctrl Pts',(0.243706194926033,1.48505200040818,-1.63195388134767));
#16402=CARTESIAN_POINT('Ctrl Pts',(0.25,1.51855708359447,-1.63095064303001));
#16403=CARTESIAN_POINT('Ctrl Pts',(0.25,1.58144291640553,-1.63095064303001));
#16404=CARTESIAN_POINT('Ctrl Pts',(0.243706194926033,1.61494799959182,-1.63195388134767));
#16405=CARTESIAN_POINT('Ctrl Pts',(0.218177859368546,1.67652816181843,-1.63556247215209));
#16406=CARTESIAN_POINT('Ctrl Pts',(0.198945932189457,1.70460745840382,-1.63811406745469));
#16407=CARTESIAN_POINT('Ctrl Pts',(0.154607860978349,1.74894552961493,-1.64289183246942));
#16408=CARTESIAN_POINT('Ctrl Pts',(0.126528390765307,1.76817777258318,-1.64543058688707));
#16409=CARTESIAN_POINT('Ctrl Pts',(0.0649476351123398,1.79370633789704,
-1.64900971937348));
#16410=CARTESIAN_POINT('Ctrl Pts',(0.031442345428849,1.8,-1.65));
#16411=CARTESIAN_POINT('Ctrl Pts',(7.63278329429795E-17,1.8,-1.65));
#16412=CARTESIAN_POINT('',(-0.25,1.55,-1.63095064303001));
#16413=CARTESIAN_POINT('Ctrl Pts',(9.0205620750794E-17,1.8,-1.65));
#16414=CARTESIAN_POINT('Ctrl Pts',(-0.0314423454288488,1.8,-1.65));
#16415=CARTESIAN_POINT('Ctrl Pts',(-0.0649476351123396,1.79370633789704,
-1.64900971937348));
#16416=CARTESIAN_POINT('Ctrl Pts',(-0.126528390765307,1.76817777258318,
-1.64543058688707));
#16417=CARTESIAN_POINT('Ctrl Pts',(-0.154607860978348,1.74894552961493,
-1.64289183246942));
#16418=CARTESIAN_POINT('Ctrl Pts',(-0.198945932189456,1.70460745840382,
-1.63811406745469));
#16419=CARTESIAN_POINT('Ctrl Pts',(-0.218177859368546,1.67652816181843,
-1.63556247215209));
#16420=CARTESIAN_POINT('Ctrl Pts',(-0.243706194926033,1.61494799959182,
-1.63195388134767));
#16421=CARTESIAN_POINT('Ctrl Pts',(-0.25,1.58144291640553,-1.63095064303001));
#16422=CARTESIAN_POINT('Ctrl Pts',(-0.25,1.55,-1.63095064303001));
#16423=CARTESIAN_POINT('Ctrl Pts',(-0.25,1.55,-1.63095064303001));
#16424=CARTESIAN_POINT('Ctrl Pts',(-0.25,1.51855708359447,-1.63095064303001));
#16425=CARTESIAN_POINT('Ctrl Pts',(-0.243706194926033,1.48505200040818,
-1.63195388134767));
#16426=CARTESIAN_POINT('Ctrl Pts',(-0.218177859368546,1.42347183818157,
-1.63556247215209));
#16427=CARTESIAN_POINT('Ctrl Pts',(-0.198945932189457,1.39539254159618,
-1.63811406745469));
#16428=CARTESIAN_POINT('Ctrl Pts',(-0.154607860978349,1.35105447038507,
-1.64289183246942));
#16429=CARTESIAN_POINT('Ctrl Pts',(-0.126528390765307,1.33182222741682,
-1.64543058688707));
#16430=CARTESIAN_POINT('Ctrl Pts',(-0.0649476351123398,1.30629366210296,
-1.64900971937348));
#16431=CARTESIAN_POINT('Ctrl Pts',(-0.031442345428849,1.3,-1.65));
#16432=CARTESIAN_POINT('Ctrl Pts',(-4.85722573273506E-17,1.3,-1.65));
#16433=CARTESIAN_POINT('',(0.,1.8,1.65));
#16434=CARTESIAN_POINT('',(0.,1.3,1.65));
#16435=CARTESIAN_POINT('Ctrl Pts',(8.32667268468867E-17,1.8,1.65));
#16436=CARTESIAN_POINT('Ctrl Pts',(0.031442345428849,1.8,1.65));
#16437=CARTESIAN_POINT('Ctrl Pts',(0.0649476351123398,1.79370633789704,
1.64900971937348));
#16438=CARTESIAN_POINT('Ctrl Pts',(0.126528390765307,1.76817777258318,1.64543058688707));
#16439=CARTESIAN_POINT('Ctrl Pts',(0.154607860978349,1.74894552961493,1.64289183246942));
#16440=CARTESIAN_POINT('Ctrl Pts',(0.198945932189457,1.70460745840382,1.63811406745469));
#16441=CARTESIAN_POINT('Ctrl Pts',(0.218177859368546,1.67652816181843,1.63556247215209));
#16442=CARTESIAN_POINT('Ctrl Pts',(0.243706194926033,1.61494799959182,1.63195388134767));
#16443=CARTESIAN_POINT('Ctrl Pts',(0.25,1.58144291640553,1.63095064303001));
#16444=CARTESIAN_POINT('Ctrl Pts',(0.25,1.51855708359447,1.63095064303001));
#16445=CARTESIAN_POINT('Ctrl Pts',(0.243706194926033,1.48505200040818,1.63195388134767));
#16446=CARTESIAN_POINT('Ctrl Pts',(0.218177859368546,1.42347183818157,1.63556247215209));
#16447=CARTESIAN_POINT('Ctrl Pts',(0.198945932189457,1.39539254159618,1.63811406745469));
#16448=CARTESIAN_POINT('Ctrl Pts',(0.154607860978348,1.35105447038507,1.64289183246942));
#16449=CARTESIAN_POINT('Ctrl Pts',(0.126528390765307,1.33182222741682,1.64543058688707));
#16450=CARTESIAN_POINT('Ctrl Pts',(0.0649476351123397,1.30629366210296,
1.64900971937348));
#16451=CARTESIAN_POINT('Ctrl Pts',(0.0314423454288488,1.3,1.65));
#16452=CARTESIAN_POINT('Ctrl Pts',(-1.38777878078145E-17,1.3,1.65));
#16453=CARTESIAN_POINT('',(-0.25,1.55,1.63095064303001));
#16454=CARTESIAN_POINT('Ctrl Pts',(-5.55111512312578E-17,1.3,1.65));
#16455=CARTESIAN_POINT('Ctrl Pts',(-0.031442345428849,1.3,1.65));
#16456=CARTESIAN_POINT('Ctrl Pts',(-0.0649476351123398,1.30629366210296,
1.64900971937348));
#16457=CARTESIAN_POINT('Ctrl Pts',(-0.126528390765307,1.33182222741682,
1.64543058688707));
#16458=CARTESIAN_POINT('Ctrl Pts',(-0.154607860978349,1.35105447038507,
1.64289183246942));
#16459=CARTESIAN_POINT('Ctrl Pts',(-0.198945932189457,1.39539254159618,
1.63811406745469));
#16460=CARTESIAN_POINT('Ctrl Pts',(-0.218177859368546,1.42347183818157,
1.63556247215209));
#16461=CARTESIAN_POINT('Ctrl Pts',(-0.243706194926033,1.48505200040818,
1.63195388134767));
#16462=CARTESIAN_POINT('Ctrl Pts',(-0.25,1.51855708359447,1.63095064303001));
#16463=CARTESIAN_POINT('Ctrl Pts',(-0.25,1.55,1.63095064303001));
#16464=CARTESIAN_POINT('Ctrl Pts',(-0.25,1.55,1.63095064303001));
#16465=CARTESIAN_POINT('Ctrl Pts',(-0.25,1.58144291640553,1.63095064303001));
#16466=CARTESIAN_POINT('Ctrl Pts',(-0.243706194926033,1.61494799959182,
1.63195388134767));
#16467=CARTESIAN_POINT('Ctrl Pts',(-0.218177859368546,1.67652816181843,
1.63556247215209));
#16468=CARTESIAN_POINT('Ctrl Pts',(-0.198945932189456,1.70460745840382,
1.63811406745469));
#16469=CARTESIAN_POINT('Ctrl Pts',(-0.154607860978348,1.74894552961493,
1.64289183246942));
#16470=CARTESIAN_POINT('Ctrl Pts',(-0.126528390765307,1.76817777258318,
1.64543058688707));
#16471=CARTESIAN_POINT('Ctrl Pts',(-0.0649476351123396,1.79370633789704,
1.64900971937348));
#16472=CARTESIAN_POINT('Ctrl Pts',(-0.0314423454288488,1.8,1.65));
#16473=CARTESIAN_POINT('Ctrl Pts',(7.63278329429795E-17,1.8,1.65));
#16474=CARTESIAN_POINT('Origin',(0.,1.55,0.));
#16475=CARTESIAN_POINT('',(-0.34736109069228,1.55,0.489224153812002));
#16476=CARTESIAN_POINT('',(0.125,1.55,0.21650635094611));
#16477=CARTESIAN_POINT('Ctrl Pts',(-0.34736109069228,1.55,0.489224153812002));
#16478=CARTESIAN_POINT('Ctrl Pts',(-0.34736109069228,1.58183602855499,0.489224153812002));
#16479=CARTESIAN_POINT('Ctrl Pts',(-0.353251858758695,1.61548166177648,
0.485186294875824));
#16480=CARTESIAN_POINT('Ctrl Pts',(-0.375307371004242,1.67693412158597,
0.468334260082228));
#16481=CARTESIAN_POINT('Ctrl Pts',(-0.391292050254279,1.70478184753241,
0.455434178332924));
#16482=CARTESIAN_POINT('Ctrl Pts',(-0.425012071836758,1.74874496453875,
0.424138206994599));
#16483=CARTESIAN_POINT('Ctrl Pts',(-0.445091520936419,1.76792916820474,
0.403563860606914));
#16484=CARTESIAN_POINT('Ctrl Pts',(-0.484488022261587,1.79356669468566,
0.355304950761552));
#16485=CARTESIAN_POINT('Ctrl Pts',(-0.503716463284046,1.8,0.32753749298313));
#16486=CARTESIAN_POINT('Ctrl Pts',(-0.535514021257281,1.8,0.27246250701687));
#16487=CARTESIAN_POINT('Ctrl Pts',(-0.549947124580677,1.79356669468566,
0.241926459727038));
#16488=CARTESIAN_POINT('Ctrl Pts',(-0.572042315803119,1.76792916820474,
0.183678633836535));
#16489=CARTESIAN_POINT('Ctrl Pts',(-0.579820497891285,1.74874496453875,
0.156002147628389));
#16490=CARTESIAN_POINT('Ctrl Pts',(-0.590063593315144,1.70478184753241,
0.11115176665264));
#16491=CARTESIAN_POINT('Ctrl Pts',(-0.593243052195919,1.67693412158597,
0.0908585874761102));
#16492=CARTESIAN_POINT('Ctrl Pts',(-0.596809586309859,1.61548166177648,
0.0633319361811903));
#16493=CARTESIAN_POINT('Ctrl Pts',(-0.59736109069228,1.58183602855499,0.0562114519197831));
#16494=CARTESIAN_POINT('Ctrl Pts',(-0.59736109069228,1.51816397144501,0.0562114519197831));
#16495=CARTESIAN_POINT('Ctrl Pts',(-0.596809586309859,1.48451833822352,
0.0633319361811902));
#16496=CARTESIAN_POINT('Ctrl Pts',(-0.593243052195919,1.42306587841403,
0.0908585874761101));
#16497=CARTESIAN_POINT('Ctrl Pts',(-0.590063593315144,1.39521815246759,
0.11115176665264));
#16498=CARTESIAN_POINT('Ctrl Pts',(-0.579820497891285,1.35125503546125,
0.156002147628389));
#16499=CARTESIAN_POINT('Ctrl Pts',(-0.572042315803119,1.33207083179526,
0.183678633836535));
#16500=CARTESIAN_POINT('Ctrl Pts',(-0.549947124580676,1.30643330531434,
0.241926459727038));
#16501=CARTESIAN_POINT('Ctrl Pts',(-0.535514021257281,1.3,0.27246250701687));
#16502=CARTESIAN_POINT('Ctrl Pts',(-0.503716463284046,1.3,0.32753749298313));
#16503=CARTESIAN_POINT('Ctrl Pts',(-0.484488022261587,1.30643330531434,
0.355304950761552));
#16504=CARTESIAN_POINT('Ctrl Pts',(-0.445091520936419,1.33207083179526,
0.403563860606914));
#16505=CARTESIAN_POINT('Ctrl Pts',(-0.425012071836758,1.35125503546125,
0.424138206994599));
#16506=CARTESIAN_POINT('Ctrl Pts',(-0.391292050254279,1.39521815246759,
0.455434178332924));
#16507=CARTESIAN_POINT('Ctrl Pts',(-0.375307371004241,1.42306587841403,
0.468334260082228));
#16508=CARTESIAN_POINT('Ctrl Pts',(-0.353251858758695,1.48451833822352,
0.485186294875824));
#16509=CARTESIAN_POINT('Ctrl Pts',(-0.34736109069228,1.51816397144501,0.489224153812002));
#16510=CARTESIAN_POINT('Ctrl Pts',(-0.34736109069228,1.55,0.489224153812002));
#16511=CARTESIAN_POINT('Origin',(0.,1.55,0.));
#16512=CARTESIAN_POINT('',(0.59736109069228,1.55,-0.0562114519197831));
#16513=CARTESIAN_POINT('Ctrl Pts',(0.59736109069228,1.55,-0.0562114519197831));
#16514=CARTESIAN_POINT('Ctrl Pts',(0.59736109069228,1.51816397144501,-0.0562114519197831));
#16515=CARTESIAN_POINT('Ctrl Pts',(0.596809586309859,1.48451833822352,-0.0633319361811902));
#16516=CARTESIAN_POINT('Ctrl Pts',(0.593243052195919,1.42306587841403,-0.0908585874761101));
#16517=CARTESIAN_POINT('Ctrl Pts',(0.590063593315144,1.39521815246759,-0.11115176665264));
#16518=CARTESIAN_POINT('Ctrl Pts',(0.579820497891285,1.35125503546125,-0.156002147628389));
#16519=CARTESIAN_POINT('Ctrl Pts',(0.572042315803119,1.33207083179526,-0.183678633836535));
#16520=CARTESIAN_POINT('Ctrl Pts',(0.549947124580677,1.30643330531434,-0.241926459727038));
#16521=CARTESIAN_POINT('Ctrl Pts',(0.535514021257281,1.3,-0.27246250701687));
#16522=CARTESIAN_POINT('Ctrl Pts',(0.503716463284046,1.3,-0.32753749298313));
#16523=CARTESIAN_POINT('Ctrl Pts',(0.484488022261587,1.30643330531434,-0.355304950761552));
#16524=CARTESIAN_POINT('Ctrl Pts',(0.445091520936419,1.33207083179526,-0.403563860606914));
#16525=CARTESIAN_POINT('Ctrl Pts',(0.425012071836758,1.35125503546125,-0.424138206994599));
#16526=CARTESIAN_POINT('Ctrl Pts',(0.391292050254279,1.39521815246759,-0.455434178332924));
#16527=CARTESIAN_POINT('Ctrl Pts',(0.375307371004241,1.42306587841403,-0.468334260082228));
#16528=CARTESIAN_POINT('Ctrl Pts',(0.353251858758695,1.48451833822352,-0.485186294875824));
#16529=CARTESIAN_POINT('Ctrl Pts',(0.34736109069228,1.51816397144501,-0.489224153812002));
#16530=CARTESIAN_POINT('Ctrl Pts',(0.34736109069228,1.58183602855499,-0.489224153812002));
#16531=CARTESIAN_POINT('Ctrl Pts',(0.353251858758695,1.61548166177647,-0.485186294875824));
#16532=CARTESIAN_POINT('Ctrl Pts',(0.375307371004241,1.67693412158597,-0.468334260082228));
#16533=CARTESIAN_POINT('Ctrl Pts',(0.391292050254279,1.70478184753241,-0.455434178332924));
#16534=CARTESIAN_POINT('Ctrl Pts',(0.425012071836758,1.74874496453875,-0.424138206994599));
#16535=CARTESIAN_POINT('Ctrl Pts',(0.445091520936419,1.76792916820474,-0.403563860606914));
#16536=CARTESIAN_POINT('Ctrl Pts',(0.484488022261587,1.79356669468566,-0.355304950761552));
#16537=CARTESIAN_POINT('Ctrl Pts',(0.503716463284046,1.8,-0.32753749298313));
#16538=CARTESIAN_POINT('Ctrl Pts',(0.535514021257281,1.8,-0.27246250701687));
#16539=CARTESIAN_POINT('Ctrl Pts',(0.549947124580677,1.79356669468566,-0.241926459727038));
#16540=CARTESIAN_POINT('Ctrl Pts',(0.572042315803119,1.76792916820474,-0.183678633836535));
#16541=CARTESIAN_POINT('Ctrl Pts',(0.579820497891285,1.74874496453875,-0.156002147628389));
#16542=CARTESIAN_POINT('Ctrl Pts',(0.590063593315144,1.70478184753241,-0.111151766652641));
#16543=CARTESIAN_POINT('Ctrl Pts',(0.593243052195919,1.67693412158597,-0.0908585874761104));
#16544=CARTESIAN_POINT('Ctrl Pts',(0.596809586309859,1.61548166177648,-0.0633319361811903));
#16545=CARTESIAN_POINT('Ctrl Pts',(0.59736109069228,1.58183602855499,-0.0562114519197831));
#16546=CARTESIAN_POINT('Ctrl Pts',(0.59736109069228,1.55,-0.0562114519197831));
#16547=CARTESIAN_POINT('',(0.125,1.55,0.21650635094611));
#16548=CARTESIAN_POINT('Origin',(0.,1.55,0.));
#16549=CARTESIAN_POINT('',(-0.25,1.55,-0.545435605731786));
#16550=CARTESIAN_POINT('',(-0.25,1.55,0.));
#16551=CARTESIAN_POINT('Ctrl Pts',(-0.25,1.55,-0.545435605731786));
#16552=CARTESIAN_POINT('Ctrl Pts',(-0.25,1.58183602855499,-0.545435605731786));
#16553=CARTESIAN_POINT('Ctrl Pts',(-0.243557727551164,1.61548166177648,
-0.548518231057014));
#16554=CARTESIAN_POINT('Ctrl Pts',(-0.217935681191677,1.67693412158597,
-0.559192847558338));
#16555=CARTESIAN_POINT('Ctrl Pts',(-0.198771543060865,1.70478184753241,
-0.566585944985565));
#16556=CARTESIAN_POINT('Ctrl Pts',(-0.154808426054527,1.74874496453875,
-0.580140354622989));
#16557=CARTESIAN_POINT('Ctrl Pts',(-0.1269507948667,1.76792916820474,-0.587242494443449));
#16558=CARTESIAN_POINT('Ctrl Pts',(-0.0654591023190899,1.79356669468566,
-0.597231410488591));
#16559=CARTESIAN_POINT('Ctrl Pts',(-0.0317975579732349,1.8,-0.6));
#16560=CARTESIAN_POINT('Ctrl Pts',(0.0317975579732349,1.8,-0.6));
#16561=CARTESIAN_POINT('Ctrl Pts',(0.0654591023190898,1.79356669468566,
-0.597231410488591));
#16562=CARTESIAN_POINT('Ctrl Pts',(0.1269507948667,1.76792916820474,-0.587242494443449));
#16563=CARTESIAN_POINT('Ctrl Pts',(0.154808426054527,1.74874496453875,-0.580140354622989));
#16564=CARTESIAN_POINT('Ctrl Pts',(0.198771543060865,1.70478184753241,-0.566585944985565));
#16565=CARTESIAN_POINT('Ctrl Pts',(0.217935681191677,1.67693412158597,-0.559192847558338));
#16566=CARTESIAN_POINT('Ctrl Pts',(0.243557727551164,1.61548166177648,-0.548518231057014));
#16567=CARTESIAN_POINT('Ctrl Pts',(0.25,1.58183602855499,-0.545435605731786));
#16568=CARTESIAN_POINT('Ctrl Pts',(0.25,1.51816397144501,-0.545435605731786));
#16569=CARTESIAN_POINT('Ctrl Pts',(0.243557727551164,1.48451833822352,-0.548518231057014));
#16570=CARTESIAN_POINT('Ctrl Pts',(0.217935681191677,1.42306587841403,-0.559192847558338));
#16571=CARTESIAN_POINT('Ctrl Pts',(0.198771543060865,1.39521815246759,-0.566585944985565));
#16572=CARTESIAN_POINT('Ctrl Pts',(0.154808426054527,1.35125503546125,-0.580140354622989));
#16573=CARTESIAN_POINT('Ctrl Pts',(0.1269507948667,1.33207083179526,-0.587242494443449));
#16574=CARTESIAN_POINT('Ctrl Pts',(0.0654591023190899,1.30643330531434,
-0.597231410488591));
#16575=CARTESIAN_POINT('Ctrl Pts',(0.0317975579732349,1.3,-0.6));
#16576=CARTESIAN_POINT('Ctrl Pts',(-0.0317975579732349,1.3,-0.6));
#16577=CARTESIAN_POINT('Ctrl Pts',(-0.0654591023190899,1.30643330531434,
-0.597231410488591));
#16578=CARTESIAN_POINT('Ctrl Pts',(-0.1269507948667,1.33207083179526,-0.587242494443449));
#16579=CARTESIAN_POINT('Ctrl Pts',(-0.154808426054527,1.35125503546125,
-0.580140354622989));
#16580=CARTESIAN_POINT('Ctrl Pts',(-0.198771543060865,1.39521815246759,
-0.566585944985565));
#16581=CARTESIAN_POINT('Ctrl Pts',(-0.217935681191677,1.42306587841403,
-0.559192847558338));
#16582=CARTESIAN_POINT('Ctrl Pts',(-0.243557727551164,1.48451833822352,
-0.548518231057014));
#16583=CARTESIAN_POINT('Ctrl Pts',(-0.25,1.51816397144501,-0.545435605731786));
#16584=CARTESIAN_POINT('Ctrl Pts',(-0.25,1.55,-0.545435605731786));
#16585=CARTESIAN_POINT('Origin',(0.,1.55,0.));
#16586=CARTESIAN_POINT('',(-0.25,1.55,0.545435605731786));
#16587=CARTESIAN_POINT('Ctrl Pts',(-0.25,1.55,0.545435605731786));
#16588=CARTESIAN_POINT('Ctrl Pts',(-0.25,1.51816397144501,0.545435605731786));
#16589=CARTESIAN_POINT('Ctrl Pts',(-0.243557727551164,1.48451833822352,
0.548518231057014));
#16590=CARTESIAN_POINT('Ctrl Pts',(-0.217935681191677,1.42306587841403,
0.559192847558338));
#16591=CARTESIAN_POINT('Ctrl Pts',(-0.198771543060865,1.39521815246759,
0.566585944985565));
#16592=CARTESIAN_POINT('Ctrl Pts',(-0.154808426054527,1.35125503546125,
0.580140354622989));
#16593=CARTESIAN_POINT('Ctrl Pts',(-0.1269507948667,1.33207083179526,0.587242494443449));
#16594=CARTESIAN_POINT('Ctrl Pts',(-0.0654591023190899,1.30643330531434,
0.597231410488591));
#16595=CARTESIAN_POINT('Ctrl Pts',(-0.0317975579732349,1.3,0.6));
#16596=CARTESIAN_POINT('Ctrl Pts',(0.0317975579732349,1.3,0.6));
#16597=CARTESIAN_POINT('Ctrl Pts',(0.0654591023190899,1.30643330531434,
0.597231410488591));
#16598=CARTESIAN_POINT('Ctrl Pts',(0.1269507948667,1.33207083179526,0.587242494443449));
#16599=CARTESIAN_POINT('Ctrl Pts',(0.154808426054527,1.35125503546125,0.580140354622989));
#16600=CARTESIAN_POINT('Ctrl Pts',(0.198771543060865,1.39521815246759,0.566585944985565));
#16601=CARTESIAN_POINT('Ctrl Pts',(0.217935681191677,1.42306587841403,0.559192847558338));
#16602=CARTESIAN_POINT('Ctrl Pts',(0.243557727551164,1.48451833822352,0.548518231057014));
#16603=CARTESIAN_POINT('Ctrl Pts',(0.25,1.51816397144501,0.545435605731786));
#16604=CARTESIAN_POINT('Ctrl Pts',(0.25,1.58183602855499,0.545435605731786));
#16605=CARTESIAN_POINT('Ctrl Pts',(0.243557727551164,1.61548166177648,0.548518231057014));
#16606=CARTESIAN_POINT('Ctrl Pts',(0.217935681191677,1.67693412158597,0.559192847558338));
#16607=CARTESIAN_POINT('Ctrl Pts',(0.198771543060865,1.70478184753241,0.566585944985565));
#16608=CARTESIAN_POINT('Ctrl Pts',(0.154808426054527,1.74874496453875,0.580140354622989));
#16609=CARTESIAN_POINT('Ctrl Pts',(0.1269507948667,1.76792916820474,0.587242494443449));
#16610=CARTESIAN_POINT('Ctrl Pts',(0.0654591023190898,1.79356669468566,
0.597231410488591));
#16611=CARTESIAN_POINT('Ctrl Pts',(0.0317975579732349,1.8,0.6));
#16612=CARTESIAN_POINT('Ctrl Pts',(-0.0317975579732349,1.8,0.6));
#16613=CARTESIAN_POINT('Ctrl Pts',(-0.0654591023190898,1.79356669468566,
0.597231410488591));
#16614=CARTESIAN_POINT('Ctrl Pts',(-0.1269507948667,1.76792916820474,0.587242494443449));
#16615=CARTESIAN_POINT('Ctrl Pts',(-0.154808426054527,1.74874496453875,
0.580140354622989));
#16616=CARTESIAN_POINT('Ctrl Pts',(-0.198771543060865,1.70478184753241,
0.566585944985565));
#16617=CARTESIAN_POINT('Ctrl Pts',(-0.217935681191677,1.67693412158597,
0.559192847558339));
#16618=CARTESIAN_POINT('Ctrl Pts',(-0.243557727551164,1.61548166177648,
0.548518231057014));
#16619=CARTESIAN_POINT('Ctrl Pts',(-0.25,1.58183602855499,0.545435605731786));
#16620=CARTESIAN_POINT('Ctrl Pts',(-0.25,1.55,0.545435605731786));
#16621=CARTESIAN_POINT('',(-0.25,1.55,0.));
#16622=CARTESIAN_POINT('Origin',(1.65,2.25,0.));
#16623=CARTESIAN_POINT('',(-0.6,2.25,-7.34788079488412E-17));
#16624=CARTESIAN_POINT('Origin',(0.,2.25,0.));
#16625=CARTESIAN_POINT('Origin',(1.75,0.85,0.));
#16626=CARTESIAN_POINT('',(-1.75,0.85,-2.14313189850787E-16));
#16627=CARTESIAN_POINT('Origin',(0.,0.85,0.));
#16628=CARTESIAN_POINT('Origin',(0.,0.,0.));
#16629=CARTESIAN_POINT('',(-1.75,-0.85,-2.14313189850787E-16));
#16630=CARTESIAN_POINT('Origin',(0.,-0.85,0.));
#16631=CARTESIAN_POINT('',(-1.75,0.,-2.14313189850787E-16));
#16632=CARTESIAN_POINT('Origin',(0.6,-0.85,0.));
#16633=CARTESIAN_POINT('',(-0.6,-0.85,-7.34788079488412E-17));
#16634=CARTESIAN_POINT('Origin',(0.,-0.85,0.));
#16635=CARTESIAN_POINT('Origin',(0.,0.7,0.));
#16636=CARTESIAN_POINT('',(-0.6,0.7,-7.34788079488412E-17));
#16637=CARTESIAN_POINT('',(0.,0.,0.));
#16638=CARTESIAN_POINT('',(0.,0.,0.));
#16639=CARTESIAN_POINT('',(0.,0.,0.));
#16640=CARTESIAN_POINT('Origin',(0.,0.,0.));
#16641=CARTESIAN_POINT('',(-0.42,0.16,5.14351655641888E-17));
#16642=CARTESIAN_POINT('Origin',(0.,0.16,0.));
#16643=CARTESIAN_POINT('',(-0.42,0.,5.14351655641888E-17));
#16644=CARTESIAN_POINT('',(-0.42,0.,5.14351655641888E-17));
#16645=CARTESIAN_POINT('Origin',(0.,0.,0.));
#16646=CARTESIAN_POINT('Origin',(0.,0.,0.));
#16647=CARTESIAN_POINT('',(-0.8,0.16,9.79717439317883E-17));
#16648=CARTESIAN_POINT('Origin',(0.,0.16,0.));
#16649=CARTESIAN_POINT('',(-0.8,0.,9.79717439317883E-17));
#16650=CARTESIAN_POINT('',(-0.8,0.,9.79717439317883E-17));
#16651=CARTESIAN_POINT('Origin',(0.,0.,0.));
#16652=CARTESIAN_POINT('Origin',(0.,0.16,0.));
#16653=CARTESIAN_POINT('Origin',(0.,0.,0.));
#16654=CARTESIAN_POINT('',(0.,0.,0.));
#16655=CARTESIAN_POINT('Origin',(0.173205080756888,-0.8,-0.3));
#16656=CARTESIAN_POINT('',(0.346410161513775,-0.8,0.));
#16657=CARTESIAN_POINT('',(0.173205080756888,-0.8,-0.3));
#16658=CARTESIAN_POINT('',(0.346410161513775,-0.8,0.));
#16659=CARTESIAN_POINT('',(0.173205080756888,-1.28,-0.3));
#16660=CARTESIAN_POINT('',(0.173205080756888,-0.8,-0.3));
#16661=CARTESIAN_POINT('',(0.346410161513775,-1.28,0.));
#16662=CARTESIAN_POINT('',(0.346410161513775,-1.28,0.));
#16663=CARTESIAN_POINT('',(0.346410161513775,-0.8,0.));
#16664=CARTESIAN_POINT('Origin',(-0.173205080756888,-0.8,-0.3));
#16665=CARTESIAN_POINT('',(-0.173205080756888,-0.8,-0.3));
#16666=CARTESIAN_POINT('',(0.173205080756888,-0.8,-0.3));
#16667=CARTESIAN_POINT('',(-0.173205080756888,-1.28,-0.3));
#16668=CARTESIAN_POINT('',(-0.173205080756888,-0.8,-0.3));
#16669=CARTESIAN_POINT('',(0.173205080756888,-1.28,-0.3));
#16670=CARTESIAN_POINT('Origin',(-0.346410161513775,-0.8,-5.55111512312578E-17));
#16671=CARTESIAN_POINT('',(-0.346410161513775,-0.8,-4.24230095489963E-17));
#16672=CARTESIAN_POINT('',(-0.173205080756888,-0.8,-0.3));
#16673=CARTESIAN_POINT('',(-0.346410161513775,-1.28,-5.55111512312578E-17));
#16674=CARTESIAN_POINT('',(-0.346410161513775,-0.8,-4.24230095489963E-17));
#16675=CARTESIAN_POINT('',(-0.173205080756888,-1.28,-0.3));
#16676=CARTESIAN_POINT('Origin',(-0.173205080756888,-0.8,0.3));
#16677=CARTESIAN_POINT('',(-0.173205080756888,-0.8,0.3));
#16678=CARTESIAN_POINT('',(-0.346410161513775,-0.8,-4.24230095489963E-17));
#16679=CARTESIAN_POINT('',(-0.173205080756888,-1.28,0.3));
#16680=CARTESIAN_POINT('',(-0.173205080756888,-0.8,0.3));
#16681=CARTESIAN_POINT('',(-0.346410161513775,-1.28,-4.24230095489963E-17));
#16682=CARTESIAN_POINT('Origin',(0.173205080756888,-0.8,0.3));
#16683=CARTESIAN_POINT('',(0.173205080756888,-0.8,0.3));
#16684=CARTESIAN_POINT('',(-0.173205080756888,-0.8,0.3));
#16685=CARTESIAN_POINT('',(0.173205080756888,-1.28,0.3));
#16686=CARTESIAN_POINT('',(0.173205080756888,-0.8,0.3));
#16687=CARTESIAN_POINT('',(-0.173205080756888,-1.28,0.3));
#16688=CARTESIAN_POINT('Origin',(0.346410161513775,-0.8,0.));
#16689=CARTESIAN_POINT('',(0.173205080756888,-0.8,0.3));
#16690=CARTESIAN_POINT('',(0.173205080756888,-1.28,0.3));
#16691=CARTESIAN_POINT('Origin',(0.,-0.8,-5.55111512312578E-17));
#16692=CARTESIAN_POINT('Origin',(0.,-1.28,-5.55111512312578E-17));
#16693=CARTESIAN_POINT('Origin',(0.,-2.5,0.));
#16694=CARTESIAN_POINT('',(-0.3933,-2.5,4.81653586104654E-17));
#16695=CARTESIAN_POINT('Origin',(0.,-2.5,0.));
#16696=CARTESIAN_POINT('Origin',(0.6,0.8,0.));
#16697=CARTESIAN_POINT('',(-0.6,0.8,-7.34788079488412E-17));
#16698=CARTESIAN_POINT('Origin',(0.,0.8,0.));
#16699=CARTESIAN_POINT('Origin',(0.,0.775,0.));
#16700=CARTESIAN_POINT('',(-0.65,0.75,-7.9602041944578E-17));
#16701=CARTESIAN_POINT('Origin',(0.,0.75,0.));
#16702=CARTESIAN_POINT('',(-0.625,0.775,-7.65404249467096E-17));
#16703=CARTESIAN_POINT('Origin',(0.,0.39,0.));
#16704=CARTESIAN_POINT('',(-0.65,0.0299999999999998,-7.9602041944578E-17));
#16705=CARTESIAN_POINT('Origin',(0.,0.0299999999999998,0.));
#16706=CARTESIAN_POINT('',(-0.65,0.39,-7.9602041944578E-17));
#16707=CARTESIAN_POINT('Origin',(0.,0.0150000000000001,0.));
#16708=CARTESIAN_POINT('',(-0.62,5.89805981832114E-17,-7.59281015471359E-17));
#16709=CARTESIAN_POINT('Origin',(0.,0.,0.));
#16710=CARTESIAN_POINT('',(-0.635,0.0150000000000001,-7.77650717458569E-17));
#16711=CARTESIAN_POINT('Origin',(0.42,0.,0.));
#16712=CARTESIAN_POINT('',(-0.42,-3.46944695195361E-18,-5.14351655641888E-17));
#16713=CARTESIAN_POINT('Origin',(0.,0.,0.));
#16714=CARTESIAN_POINT('Origin',(0.,-0.02,0.));
#16715=CARTESIAN_POINT('',(-0.3933,-0.0534000000000001,4.81653586104654E-17));
#16716=CARTESIAN_POINT('Origin',(0.,-0.0534000000000001,0.));
#16717=CARTESIAN_POINT('',(-0.41,-0.02,-5.02105187650415E-17));
#16718=CARTESIAN_POINT('Origin',(0.,-1.48,0.));
#16719=CARTESIAN_POINT('',(-0.3933,-1.48,-4.81653586104654E-17));
#16720=CARTESIAN_POINT('',(0.,0.,0.));
#16721=CARTESIAN_POINT('Origin',(0.115470053837925,-0.5,-0.2));
#16722=CARTESIAN_POINT('',(0.23094010767585,-0.5,0.));
#16723=CARTESIAN_POINT('',(0.115470053837925,-0.5,-0.2));
#16724=CARTESIAN_POINT('',(0.23094010767585,-0.5,0.));
#16725=CARTESIAN_POINT('',(0.115470053837925,-0.8,-0.2));
#16726=CARTESIAN_POINT('',(0.115470053837925,-0.5,-0.2));
#16727=CARTESIAN_POINT('',(0.23094010767585,-0.8,0.));
#16728=CARTESIAN_POINT('',(0.23094010767585,-0.8,0.));
#16729=CARTESIAN_POINT('',(0.23094010767585,-0.5,0.));
#16730=CARTESIAN_POINT('Origin',(-0.115470053837925,-0.5,-0.2));
#16731=CARTESIAN_POINT('',(-0.115470053837925,-0.5,-0.2));
#16732=CARTESIAN_POINT('',(0.115470053837925,-0.5,-0.2));
#16733=CARTESIAN_POINT('',(-0.115470053837925,-0.8,-0.2));
#16734=CARTESIAN_POINT('',(-0.115470053837925,-0.5,-0.2));
#16735=CARTESIAN_POINT('',(0.115470053837925,-0.8,-0.2));
#16736=CARTESIAN_POINT('Origin',(-0.23094010767585,-0.5,-2.77555756156289E-17));
#16737=CARTESIAN_POINT('',(-0.23094010767585,-0.5,-2.82820063659975E-17));
#16738=CARTESIAN_POINT('',(-0.115470053837925,-0.5,-0.2));
#16739=CARTESIAN_POINT('',(-0.23094010767585,-0.8,-2.77555756156289E-17));
#16740=CARTESIAN_POINT('',(-0.23094010767585,-0.5,-2.82820063659975E-17));
#16741=CARTESIAN_POINT('',(-0.115470053837925,-0.8,-0.2));
#16742=CARTESIAN_POINT('Origin',(-0.115470053837925,-0.5,0.2));
#16743=CARTESIAN_POINT('',(-0.115470053837925,-0.5,0.2));
#16744=CARTESIAN_POINT('',(-0.23094010767585,-0.5,-2.82820063659975E-17));
#16745=CARTESIAN_POINT('',(-0.115470053837925,-0.8,0.2));
#16746=CARTESIAN_POINT('',(-0.115470053837925,-0.5,0.2));
#16747=CARTESIAN_POINT('',(-0.23094010767585,-0.8,-2.82820063659975E-17));
#16748=CARTESIAN_POINT('Origin',(0.115470053837925,-0.5,0.2));
#16749=CARTESIAN_POINT('',(0.115470053837925,-0.5,0.2));
#16750=CARTESIAN_POINT('',(-0.115470053837925,-0.5,0.2));
#16751=CARTESIAN_POINT('',(0.115470053837925,-0.8,0.2));
#16752=CARTESIAN_POINT('',(0.115470053837925,-0.5,0.2));
#16753=CARTESIAN_POINT('',(-0.115470053837925,-0.8,0.2));
#16754=CARTESIAN_POINT('Origin',(0.23094010767585,-0.5,0.));
#16755=CARTESIAN_POINT('',(0.115470053837925,-0.5,0.2));
#16756=CARTESIAN_POINT('',(0.115470053837925,-0.8,0.2));
#16757=CARTESIAN_POINT('Origin',(0.,-0.5,0.));
#16758=CARTESIAN_POINT('Origin',(0.,-0.8,0.));
#16759=CARTESIAN_POINT('Origin',(0.,-1.4,0.));
#16760=CARTESIAN_POINT('',(-0.24505,-1.4,3.00099698131059E-17));
#16761=CARTESIAN_POINT('Origin',(0.,-1.4,0.));
#16762=CARTESIAN_POINT('Origin',(0.375,0.5,0.));
#16763=CARTESIAN_POINT('',(-0.375,0.5,-4.59242549680257E-17));
#16764=CARTESIAN_POINT('Origin',(0.,0.5,0.));
#16765=CARTESIAN_POINT('Origin',(0.,0.475,0.));
#16766=CARTESIAN_POINT('',(-0.425,0.45,-5.20474889637625E-17));
#16767=CARTESIAN_POINT('Origin',(0.,0.45,0.));
#16768=CARTESIAN_POINT('',(-0.4,0.475,-4.89858719658941E-17));
#16769=CARTESIAN_POINT('Origin',(0.,0.24,0.));
#16770=CARTESIAN_POINT('',(-0.425,0.0299999999999998,-5.20474889637625E-17));
#16771=CARTESIAN_POINT('Origin',(0.,0.0299999999999998,0.));
#16772=CARTESIAN_POINT('',(-0.425,0.24,-5.20474889637625E-17));
#16773=CARTESIAN_POINT('Origin',(0.,0.0150000000000001,0.));
#16774=CARTESIAN_POINT('',(-0.395,4.85722573273506E-17,-4.83735485663204E-17));
#16775=CARTESIAN_POINT('Origin',(0.,0.,0.));
#16776=CARTESIAN_POINT('',(-0.41,0.0150000000000001,-5.02105187650415E-17));
#16777=CARTESIAN_POINT('Origin',(0.27,0.,0.));
#16778=CARTESIAN_POINT('',(-0.27,0.,-3.30654635769785E-17));
#16779=CARTESIAN_POINT('Origin',(0.,0.,0.));
#16780=CARTESIAN_POINT('Origin',(0.,-0.02,0.));
#16781=CARTESIAN_POINT('',(-0.24505,-0.0498999999999999,3.00099698131059E-17));
#16782=CARTESIAN_POINT('Origin',(0.,-0.0498999999999999,0.));
#16783=CARTESIAN_POINT('',(-0.26,-0.02,-3.18408167778312E-17));
#16784=CARTESIAN_POINT('Origin',(0.,-0.995,0.));
#16785=CARTESIAN_POINT('',(-0.24505,-0.995,-3.00099698131059E-17));
#16786=CARTESIAN_POINT('',(0.,0.,0.));
#16787=CARTESIAN_POINT('',(0.,0.,0.));
#16788=CARTESIAN_POINT('',(0.,0.,0.));
#16789=CARTESIAN_POINT('',(0.,0.,0.));
#16790=CARTESIAN_POINT('',(0.,0.,0.));
#16791=CARTESIAN_POINT('',(0.,0.,0.));
#16792=CARTESIAN_POINT('',(0.,0.,0.));
#16793=CARTESIAN_POINT('',(0.,0.,0.));
#16794=CARTESIAN_POINT('',(0.,0.,0.));
#16795=CARTESIAN_POINT('',(0.,0.,0.));
#16796=CARTESIAN_POINT('',(0.,0.,0.));
#16797=CARTESIAN_POINT('',(0.,0.,0.));
#16798=CARTESIAN_POINT('',(0.,0.,0.));
#16799=CARTESIAN_POINT('',(0.,2.,4.22));
#16800=CARTESIAN_POINT('',(-4.75,2.,2.4));
#16801=CARTESIAN_POINT('',(-4.75,2.,2.56));
#16802=CARTESIAN_POINT('',(4.75,2.,2.4));
#16803=CARTESIAN_POINT('',(4.75,2.,2.56));
#16804=CARTESIAN_POINT('',(0.,18.,4.22));
#16805=CARTESIAN_POINT('',(-4.75,18.,2.4));
#16806=CARTESIAN_POINT('',(-4.75,18.,2.56));
#16807=CARTESIAN_POINT('',(4.75,18.,2.4));
#16808=CARTESIAN_POINT('',(4.75,18.,2.56));
#16809=CARTESIAN_POINT('',(-2.8,-9.,2.));
#16810=CARTESIAN_POINT('',(2.8,-9.,2.));
#16811=CARTESIAN_POINT('',(0.,0.,0.));
#16812=CARTESIAN_POINT('',(0.,0.,0.));
#16813=CARTESIAN_POINT('Origin',(-0.2,9.5,3.52));
#16814=CARTESIAN_POINT('',(-0.2,11.5,3.65431457505076));
#16815=CARTESIAN_POINT('',(-0.2,9.5,3.65431457505076));
#16816=CARTESIAN_POINT('',(-0.2,-3.1,3.65431457505076));
#16817=CARTESIAN_POINT('',(-0.2,11.5,3.87));
#16818=CARTESIAN_POINT('',(-0.2,11.5,3.87));
#16819=CARTESIAN_POINT('',(-0.2,9.5,3.87));
#16820=CARTESIAN_POINT('',(-0.2,9.5,3.87));
#16821=CARTESIAN_POINT('',(-0.2,9.5,3.87));
#16822=CARTESIAN_POINT('Origin',(0.,9.5,3.695));
#16823=CARTESIAN_POINT('',(0.2,9.5,3.65431457505076));
#16824=CARTESIAN_POINT('Origin',(0.,9.5,4.22));
#16825=CARTESIAN_POINT('',(0.2,9.5,3.87));
#16826=CARTESIAN_POINT('',(0.2,9.5,3.87));
#16827=CARTESIAN_POINT('',(0.2,9.5,3.52));
#16828=CARTESIAN_POINT('Origin',(0.2,9.5,3.87));
#16829=CARTESIAN_POINT('',(0.2,11.5,3.65431457505076));
#16830=CARTESIAN_POINT('',(0.2,-3.1,3.65431457505076));
#16831=CARTESIAN_POINT('',(0.2,11.5,3.87));
#16832=CARTESIAN_POINT('',(0.2,9.5,3.87));
#16833=CARTESIAN_POINT('',(0.2,11.5,3.52));
#16834=CARTESIAN_POINT('Origin',(-0.2,9.5,3.87));
#16835=CARTESIAN_POINT('',(0.2,11.5,3.87));
#16836=CARTESIAN_POINT('Origin',(0.,11.5,3.695));
#16837=CARTESIAN_POINT('Origin',(0.,11.5,4.22));
#16838=CARTESIAN_POINT('Origin',(0.,20.5,4.22));
#16839=CARTESIAN_POINT('',(-0.165,20.5,4.22));
#16840=CARTESIAN_POINT('Origin',(0.,20.5,4.22));
#16841=CARTESIAN_POINT('',(-0.165,22.,4.22));
#16842=CARTESIAN_POINT('',(-0.165,20.5,4.22));
#16843=CARTESIAN_POINT('Origin',(0.,22.,4.22));
#16844=CARTESIAN_POINT('Origin',(0.,20.5,4.22));
#16845=CARTESIAN_POINT('Origin',(0.,-3.1,4.22));
#16846=CARTESIAN_POINT('',(-0.6,22.,4.22));
#16847=CARTESIAN_POINT('Origin',(0.,22.,4.22));
#16848=CARTESIAN_POINT('',(-0.6,-3.1,4.22));
#16849=CARTESIAN_POINT('',(-0.6,-3.1,4.22));
#16850=CARTESIAN_POINT('Origin',(0.,-3.1,4.22));
#16851=CARTESIAN_POINT('Origin',(0.,22.,4.22));
#16852=CARTESIAN_POINT('Origin',(0.,-3.1,4.22));
#16853=CARTESIAN_POINT('',(0.,0.,0.));
#16854=CARTESIAN_POINT('Origin',(0.,-11.6,4.22));
#16855=CARTESIAN_POINT('',(-0.25,-5.2,4.22));
#16856=CARTESIAN_POINT('Origin',(0.,-5.2,4.22));
#16857=CARTESIAN_POINT('',(-0.25,-11.6,4.22));
#16858=CARTESIAN_POINT('',(-0.25,-11.6,4.22));
#16859=CARTESIAN_POINT('Origin',(0.,-11.6,4.22));
#16860=CARTESIAN_POINT('Origin',(0.,-5.2,4.22));
#16861=CARTESIAN_POINT('Origin',(0.,-11.6,4.22));
#16862=CARTESIAN_POINT('',(0.,0.,0.));
#16863=CARTESIAN_POINT('Origin',(0.,-5.8,4.46));
#16864=CARTESIAN_POINT('',(0.0700000000000023,-5.94941552797484,4.46));
#16865=CARTESIAN_POINT('',(0.0700000000000023,-5.65058447202516,4.46));
#16866=CARTESIAN_POINT('',(0.0700000000000023,-6.,4.46));
#16867=CARTESIAN_POINT('Origin',(0.,-5.8,4.46));
#16868=CARTESIAN_POINT('Origin',(0.,-5.8,4.46));
#16869=CARTESIAN_POINT('',(-0.0700000000000023,-5.94941552797484,4.46));
#16870=CARTESIAN_POINT('Ctrl Pts',(-0.0700000000000023,-5.94941552797484,
4.46));
#16871=CARTESIAN_POINT('Ctrl Pts',(-0.06805939906088,-5.95032468425585,
4.46056600860724));
#16872=CARTESIAN_POINT('Ctrl Pts',(-0.0660971141771659,-5.95119787419286,
4.46111278532807));
#16873=CARTESIAN_POINT('Ctrl Pts',(-0.0438689676213799,-5.9605718962209,
4.4670107091875));
#16874=CARTESIAN_POINT('Ctrl Pts',(-0.0214435590733092,-5.965,4.47));
#16875=CARTESIAN_POINT('Ctrl Pts',(0.0214435590733092,-5.965,4.47));
#16876=CARTESIAN_POINT('Ctrl Pts',(0.0438689676213799,-5.9605718962209,
4.4670107091875));
#16877=CARTESIAN_POINT('Ctrl Pts',(0.0660971141771659,-5.95119787419286,
4.46111278532807));
#16878=CARTESIAN_POINT('Ctrl Pts',(0.06805939906088,-5.95032468425585,4.46056600860724));
#16879=CARTESIAN_POINT('Ctrl Pts',(0.0700000000000023,-5.94941552797484,
4.46));
#16880=CARTESIAN_POINT('',(-0.165,-5.8,4.46));
#16881=CARTESIAN_POINT('Origin',(0.,-5.8,4.46));
#16882=CARTESIAN_POINT('',(-0.165,-5.8,4.79686653569088));
#16883=CARTESIAN_POINT('',(-0.165,-5.8,4.46));
#16884=CARTESIAN_POINT('',(0.165,-5.8,4.79686653569088));
#16885=CARTESIAN_POINT('Ctrl Pts',(0.165,-5.8,4.79686653569088));
#16886=CARTESIAN_POINT('Ctrl Pts',(0.165,-5.82083617414449,4.79686653569088));
#16887=CARTESIAN_POINT('Ctrl Pts',(0.160813813148411,-5.84298285479422,
4.79811329537163));
#16888=CARTESIAN_POINT('Ctrl Pts',(0.143942819671378,-5.88360069371169,
4.80254315455331));
#16889=CARTESIAN_POINT('Ctrl Pts',(0.13126336772609,-5.90208187006547,4.80565449242259));
#16890=CARTESIAN_POINT('Ctrl Pts',(0.102084895635736,-5.93126034215582,
4.81143878680194));
#16891=CARTESIAN_POINT('Ctrl Pts',(0.0836024737060978,-5.9439421456793,
4.81449794909247));
#16892=CARTESIAN_POINT('Ctrl Pts',(0.0429801659601906,-5.96081486463402,
4.81880705606552));
#16893=CARTESIAN_POINT('Ctrl Pts',(0.0208318535088818,-5.965,4.82));
#16894=CARTESIAN_POINT('Ctrl Pts',(-0.0208318535088819,-5.965,4.82));
#16895=CARTESIAN_POINT('Ctrl Pts',(-0.0429801659601906,-5.96081486463402,
4.81880705606552));
#16896=CARTESIAN_POINT('Ctrl Pts',(-0.0836024737060979,-5.9439421456793,
4.81449794909247));
#16897=CARTESIAN_POINT('Ctrl Pts',(-0.102084895635736,-5.93126034215582,
4.81143878680194));
#16898=CARTESIAN_POINT('Ctrl Pts',(-0.13126336772609,-5.90208187006547,
4.80565449242259));
#16899=CARTESIAN_POINT('Ctrl Pts',(-0.143942819671378,-5.88360069371169,
4.80254315455331));
#16900=CARTESIAN_POINT('Ctrl Pts',(-0.160813813148411,-5.84298285479422,
4.79811329537163));
#16901=CARTESIAN_POINT('Ctrl Pts',(-0.165,-5.82083617414449,4.79686653569088));
#16902=CARTESIAN_POINT('Ctrl Pts',(-0.165,-5.8,4.79686653569088));
#16903=CARTESIAN_POINT('Ctrl Pts',(-0.165,-5.8,4.79686653569088));
#16904=CARTESIAN_POINT('Ctrl Pts',(-0.165,-5.77916382585551,4.79686653569088));
#16905=CARTESIAN_POINT('Ctrl Pts',(-0.160813813148411,-5.75701714520578,
4.79811329537163));
#16906=CARTESIAN_POINT('Ctrl Pts',(-0.143942819671378,-5.71639930628831,
4.80254315455331));
#16907=CARTESIAN_POINT('Ctrl Pts',(-0.13126336772609,-5.69791812993453,
4.80565449242259));
#16908=CARTESIAN_POINT('Ctrl Pts',(-0.102084895635736,-5.66873965784418,
4.81143878680194));
#16909=CARTESIAN_POINT('Ctrl Pts',(-0.0836024737060979,-5.6560578543207,
4.81449794909247));
#16910=CARTESIAN_POINT('Ctrl Pts',(-0.0429801659601906,-5.63918513536598,
4.81880705606552));
#16911=CARTESIAN_POINT('Ctrl Pts',(-0.0208318535088819,-5.635,4.82));
#16912=CARTESIAN_POINT('Ctrl Pts',(0.0208318535088818,-5.635,4.82));
#16913=CARTESIAN_POINT('Ctrl Pts',(0.0429801659601906,-5.63918513536598,
4.81880705606552));
#16914=CARTESIAN_POINT('Ctrl Pts',(0.0836024737060978,-5.6560578543207,
4.81449794909247));
#16915=CARTESIAN_POINT('Ctrl Pts',(0.102084895635736,-5.66873965784418,
4.81143878680194));
#16916=CARTESIAN_POINT('Ctrl Pts',(0.13126336772609,-5.69791812993453,4.80565449242259));
#16917=CARTESIAN_POINT('Ctrl Pts',(0.143942819671378,-5.71639930628831,
4.80254315455331));
#16918=CARTESIAN_POINT('Ctrl Pts',(0.160813813148411,-5.75701714520578,
4.79811329537163));
#16919=CARTESIAN_POINT('Ctrl Pts',(0.165,-5.77916382585551,4.79686653569088));
#16920=CARTESIAN_POINT('Ctrl Pts',(0.165,-5.8,4.79686653569088));
#16921=CARTESIAN_POINT('',(-0.0700000000000023,-5.65058447202516,4.46));
#16922=CARTESIAN_POINT('Origin',(0.,-5.8,4.46));
#16923=CARTESIAN_POINT('Ctrl Pts',(0.0700000000000023,-5.65058447202516,
4.46));
#16924=CARTESIAN_POINT('Ctrl Pts',(0.0680593990608798,-5.64967531574415,
4.46056600860724));
#16925=CARTESIAN_POINT('Ctrl Pts',(0.0660971141771658,-5.64880212580714,
4.46111278532807));
#16926=CARTESIAN_POINT('Ctrl Pts',(0.0438689676213798,-5.6394281037791,
4.4670107091875));
#16927=CARTESIAN_POINT('Ctrl Pts',(0.0214435590733091,-5.635,4.47));
#16928=CARTESIAN_POINT('Ctrl Pts',(-0.0214435590733092,-5.635,4.47));
#16929=CARTESIAN_POINT('Ctrl Pts',(-0.0438689676213799,-5.6394281037791,
4.4670107091875));
#16930=CARTESIAN_POINT('Ctrl Pts',(-0.0660971141771659,-5.64880212580714,
4.46111278532807));
#16931=CARTESIAN_POINT('Ctrl Pts',(-0.0680593990608798,-5.64967531574415,
4.46056600860724));
#16932=CARTESIAN_POINT('Ctrl Pts',(-0.0700000000000023,-5.65058447202516,
4.46));
#16933=CARTESIAN_POINT('Origin',(0.,-5.8,4.46));
#16934=CARTESIAN_POINT('',(-0.0700000000000023,-6.,4.46));
#16935=CARTESIAN_POINT('Origin',(0.,-6.,4.22));
#16936=CARTESIAN_POINT('',(-0.25,-3.9,4.22));
#16937=CARTESIAN_POINT('Origin',(0.,-3.9,4.22));
#16938=CARTESIAN_POINT('',(-0.25,-6.,4.22));
#16939=CARTESIAN_POINT('',(-0.25,-6.,4.22));
#16940=CARTESIAN_POINT('Origin',(0.,-6.,4.22));
#16941=CARTESIAN_POINT('Origin',(0.,-6.,4.22));
#16942=CARTESIAN_POINT('',(-0.6,-3.9,4.22));
#16943=CARTESIAN_POINT('Origin',(0.,-3.9,4.22));
#16944=CARTESIAN_POINT('',(-0.6,-6.,4.22));
#16945=CARTESIAN_POINT('',(-0.6,-6.,4.22));
#16946=CARTESIAN_POINT('Origin',(0.,-6.,4.22));
#16947=CARTESIAN_POINT('Origin',(0.,-3.9,4.22));
#16948=CARTESIAN_POINT('Origin',(0.,-6.,4.22));
#16949=CARTESIAN_POINT('',(0.,0.,0.));
#16950=CARTESIAN_POINT('Origin',(0.,9.5,4.81));
#16951=CARTESIAN_POINT('',(0.109087121146358,9.32055641555074,4.81));
#16952=CARTESIAN_POINT('',(0.109087121146358,9.67944358444926,4.81));
#16953=CARTESIAN_POINT('',(0.109087121146358,9.,4.81));
#16954=CARTESIAN_POINT('Origin',(0.,9.5,4.81));
#16955=CARTESIAN_POINT('Origin',(0.,9.5,4.81));
#16956=CARTESIAN_POINT('',(-0.109087121146358,9.32055641555074,4.81));
#16957=CARTESIAN_POINT('Ctrl Pts',(-0.109087121146358,9.32055641555074,
4.81));
#16958=CARTESIAN_POINT('Ctrl Pts',(-0.100058962329436,9.31506802844783,
4.81166924721117));
#16959=CARTESIAN_POINT('Ctrl Pts',(-0.0905297208284663,9.31021510111871,
4.81321436338553));
#16960=CARTESIAN_POINT('Ctrl Pts',(-0.0548356965671429,9.29536302924048,
4.818057680137));
#16961=CARTESIAN_POINT('Ctrl Pts',(-0.026606099485122,9.29,4.82));
#16962=CARTESIAN_POINT('Ctrl Pts',(0.0266060994851219,9.29,4.82));
#16963=CARTESIAN_POINT('Ctrl Pts',(0.0548356965671429,9.29536302924048,
4.818057680137));
#16964=CARTESIAN_POINT('Ctrl Pts',(0.0905297208284663,9.31021510111871,
4.81321436338553));
#16965=CARTESIAN_POINT('Ctrl Pts',(0.100058962329435,9.31506802844783,4.81166924721117));
#16966=CARTESIAN_POINT('Ctrl Pts',(0.109087121146358,9.32055641555074,4.81));
#16967=CARTESIAN_POINT('',(-0.21,9.5,4.81));
#16968=CARTESIAN_POINT('Origin',(0.,9.5,4.81));
#16969=CARTESIAN_POINT('',(-0.21,9.5,5.40148212005091));
#16970=CARTESIAN_POINT('',(-0.21,9.5,4.81));
#16971=CARTESIAN_POINT('',(0.21,9.5,5.40148212005091));
#16972=CARTESIAN_POINT('Ctrl Pts',(0.21,9.5,5.40148212005091));
#16973=CARTESIAN_POINT('Ctrl Pts',(0.21,9.47357292898574,5.40148212005091));
#16974=CARTESIAN_POINT('Ctrl Pts',(0.204707379175837,9.44542244591134,5.40246056146673));
#16975=CARTESIAN_POINT('Ctrl Pts',(0.183259409780015,9.39369943044444,5.40597389417424));
#16976=CARTESIAN_POINT('Ctrl Pts',(0.167106958412512,9.37012211031416,5.40845578531258));
#16977=CARTESIAN_POINT('Ctrl Pts',(0.129878495645339,9.33289364754699,5.4130982535617));
#16978=CARTESIAN_POINT('Ctrl Pts',(0.106300916040875,9.31674072098398,5.41556345497295));
#16979=CARTESIAN_POINT('Ctrl Pts',(0.0545770066794462,9.29529240674315,
5.41903845223025));
#16980=CARTESIAN_POINT('Ctrl Pts',(0.0264262107330192,9.29,5.42));
#16981=CARTESIAN_POINT('Ctrl Pts',(-0.0264262107330192,9.29,5.42));
#16982=CARTESIAN_POINT('Ctrl Pts',(-0.0545770066794462,9.29529240674315,
5.41903845223025));
#16983=CARTESIAN_POINT('Ctrl Pts',(-0.106300916040875,9.31674072098398,
5.41556345497295));
#16984=CARTESIAN_POINT('Ctrl Pts',(-0.129878495645339,9.33289364754699,
5.4130982535617));
#16985=CARTESIAN_POINT('Ctrl Pts',(-0.167106958412512,9.37012211031416,
5.40845578531258));
#16986=CARTESIAN_POINT('Ctrl Pts',(-0.183259409780015,9.39369943044444,
5.40597389417424));
#16987=CARTESIAN_POINT('Ctrl Pts',(-0.204707379175837,9.44542244591134,
5.40246056146673));
#16988=CARTESIAN_POINT('Ctrl Pts',(-0.21,9.47357292898574,5.40148212005091));
#16989=CARTESIAN_POINT('Ctrl Pts',(-0.21,9.5,5.40148212005091));
#16990=CARTESIAN_POINT('Ctrl Pts',(-0.21,9.5,5.40148212005091));
#16991=CARTESIAN_POINT('Ctrl Pts',(-0.21,9.52642707101426,5.40148212005091));
#16992=CARTESIAN_POINT('Ctrl Pts',(-0.204707379175837,9.55457755408866,
5.40246056146673));
#16993=CARTESIAN_POINT('Ctrl Pts',(-0.183259409780015,9.60630056955556,
5.40597389417424));
#16994=CARTESIAN_POINT('Ctrl Pts',(-0.167106958412512,9.62987788968584,
5.40845578531258));
#16995=CARTESIAN_POINT('Ctrl Pts',(-0.129878495645339,9.66710635245301,
5.4130982535617));
#16996=CARTESIAN_POINT('Ctrl Pts',(-0.106300916040875,9.68325927901602,
5.41556345497295));
#16997=CARTESIAN_POINT('Ctrl Pts',(-0.0545770066794462,9.70470759325685,
5.41903845223025));
#16998=CARTESIAN_POINT('Ctrl Pts',(-0.0264262107330192,9.71,5.42));
#16999=CARTESIAN_POINT('Ctrl Pts',(0.0264262107330191,9.71,5.42));
#17000=CARTESIAN_POINT('Ctrl Pts',(0.0545770066794469,9.70470759325685,
5.41903845223025));
#17001=CARTESIAN_POINT('Ctrl Pts',(0.106300916040875,9.68325927901602,5.41556345497295));
#17002=CARTESIAN_POINT('Ctrl Pts',(0.129878495645339,9.66710635245301,5.4130982535617));
#17003=CARTESIAN_POINT('Ctrl Pts',(0.167106958412512,9.62987788968584,5.40845578531258));
#17004=CARTESIAN_POINT('Ctrl Pts',(0.183259409780016,9.60630056955556,5.40597389417424));
#17005=CARTESIAN_POINT('Ctrl Pts',(0.204707379175837,9.55457755408866,5.40246056146672));
#17006=CARTESIAN_POINT('Ctrl Pts',(0.21,9.52642707101426,5.40148212005091));
#17007=CARTESIAN_POINT('Ctrl Pts',(0.21,9.5,5.40148212005091));
#17008=CARTESIAN_POINT('',(-0.109087121146358,9.67944358444926,4.81));
#17009=CARTESIAN_POINT('Origin',(0.,9.5,4.81));
#17010=CARTESIAN_POINT('Ctrl Pts',(0.109087121146358,9.67944358444926,4.81));
#17011=CARTESIAN_POINT('Ctrl Pts',(0.100058962329434,9.68493197155217,4.81166924721117));
#17012=CARTESIAN_POINT('Ctrl Pts',(0.0905297208284663,9.68978489888129,
4.81321436338553));
#17013=CARTESIAN_POINT('Ctrl Pts',(0.054835696567143,9.70463697075952,4.818057680137));
#17014=CARTESIAN_POINT('Ctrl Pts',(0.026606099485122,9.71,4.82));
#17015=CARTESIAN_POINT('Ctrl Pts',(-0.026606099485122,9.71,4.82));
#17016=CARTESIAN_POINT('Ctrl Pts',(-0.0548356965671429,9.70463697075952,
4.818057680137));
#17017=CARTESIAN_POINT('Ctrl Pts',(-0.0905297208284662,9.68978489888129,
4.81321436338553));
#17018=CARTESIAN_POINT('Ctrl Pts',(-0.100058962329435,9.68493197155217,
4.81166924721117));
#17019=CARTESIAN_POINT('Ctrl Pts',(-0.109087121146358,9.67944358444926,
4.81));
#17020=CARTESIAN_POINT('Origin',(0.,9.5,4.81));
#17021=CARTESIAN_POINT('',(-0.109087121146358,9.,4.81));
#17022=CARTESIAN_POINT('Origin',(-0.2,8.9,3.44));
#17023=CARTESIAN_POINT('',(-0.2,9.,3.44));
#17024=CARTESIAN_POINT('',(-0.2,9.,3.65431457505076));
#17025=CARTESIAN_POINT('',(-0.2,9.,3.83));
#17026=CARTESIAN_POINT('',(-0.2,12.,3.44));
#17027=CARTESIAN_POINT('',(-0.2,8.9,3.44));
#17028=CARTESIAN_POINT('',(-0.2,12.,3.65431457505076));
#17029=CARTESIAN_POINT('',(-0.2,12.,3.83));
#17030=CARTESIAN_POINT('',(-0.2,9.,3.65431457505076));
#17031=CARTESIAN_POINT('Origin',(0.2,8.9,3.44));
#17032=CARTESIAN_POINT('',(0.2,9.,3.44));
#17033=CARTESIAN_POINT('',(0.1,9.,3.44));
#17034=CARTESIAN_POINT('',(0.2,12.,3.44));
#17035=CARTESIAN_POINT('',(0.2,8.9,3.44));
#17036=CARTESIAN_POINT('',(0.1,12.,3.44));
#17037=CARTESIAN_POINT('Origin',(0.2,8.9,4.22));
#17038=CARTESIAN_POINT('',(0.2,9.,3.65431457505076));
#17039=CARTESIAN_POINT('',(0.2,9.,4.22));
#17040=CARTESIAN_POINT('',(0.2,12.,3.65431457505076));
#17041=CARTESIAN_POINT('',(0.2,9.,3.65431457505076));
#17042=CARTESIAN_POINT('',(0.2,12.,4.22));
#17043=CARTESIAN_POINT('Origin',(0.,12.,4.22));
#17044=CARTESIAN_POINT('',(-1.2,12.,4.22));
#17045=CARTESIAN_POINT('Origin',(0.,12.,4.22));
#17046=CARTESIAN_POINT('Origin',(0.,12.,4.22));
#17047=CARTESIAN_POINT('Origin',(0.,9.,4.22));
#17048=CARTESIAN_POINT('Origin',(0.,9.,4.22));
#17049=CARTESIAN_POINT('Origin',(0.,11.,4.22));
#17050=CARTESIAN_POINT('',(-2.8,11.,4.22));
#17051=CARTESIAN_POINT('Origin',(0.,11.,4.22));
#17052=CARTESIAN_POINT('',(-1.2,11.,4.22));
#17053=CARTESIAN_POINT('Origin',(0.,11.,4.22));
#17054=CARTESIAN_POINT('Origin',(0.,10.,4.22));
#17055=CARTESIAN_POINT('',(-2.8,10.,4.22));
#17056=CARTESIAN_POINT('Origin',(0.,10.,4.22));
#17057=CARTESIAN_POINT('',(-1.2,10.,4.22));
#17058=CARTESIAN_POINT('Origin',(0.,10.,4.22));
#17059=CARTESIAN_POINT('Origin',(0.,10.,4.22));
#17060=CARTESIAN_POINT('',(-2.8,10.,4.22));
#17061=CARTESIAN_POINT('Origin',(0.,9.,4.22));
#17062=CARTESIAN_POINT('',(-1.2,9.,4.22));
#17063=CARTESIAN_POINT('',(-1.2,9.,4.22));
#17064=CARTESIAN_POINT('Origin',(0.,9.,4.22));
#17065=CARTESIAN_POINT('Origin',(0.,9.,4.22));
#17066=CARTESIAN_POINT('',(-1.2,9.,4.22));
#17067=CARTESIAN_POINT('Origin',(0.,9.,4.22));
#17068=CARTESIAN_POINT('',(0.,0.,0.));
#17069=CARTESIAN_POINT('Origin',(0.,0.75,4.81));
#17070=CARTESIAN_POINT('',(0.133884278389959,0.588213103126366,4.81));
#17071=CARTESIAN_POINT('',(0.133884278389959,0.911786896873634,4.81));
#17072=CARTESIAN_POINT('',(0.133884278389959,0.35,4.81));
#17073=CARTESIAN_POINT('Origin',(0.,0.75,4.81));
#17074=CARTESIAN_POINT('Origin',(0.,0.75,4.81));
#17075=CARTESIAN_POINT('',(-0.133884278389959,0.588213103126366,4.81));
#17076=CARTESIAN_POINT('Ctrl Pts',(-0.133884278389959,0.588213103126366,
4.81));
#17077=CARTESIAN_POINT('Ctrl Pts',(-0.118254395260805,0.575278831782373,
4.81354677224418));
#17078=CARTESIAN_POINT('Ctrl Pts',(-0.1001097876823,0.564200683412563,4.81698224789957));
#17079=CARTESIAN_POINT('Ctrl Pts',(-0.0548298721325192,0.545361438945571,
4.8230741628997));
#17080=CARTESIAN_POINT('Ctrl Pts',(-0.0266020595922903,0.54,4.825));
#17081=CARTESIAN_POINT('Ctrl Pts',(0.0266020595922903,0.54,4.825));
#17082=CARTESIAN_POINT('Ctrl Pts',(0.0548298721325192,0.545361438945571,
4.8230741628997));
#17083=CARTESIAN_POINT('Ctrl Pts',(0.1001097876823,0.564200683412563,4.81698224789957));
#17084=CARTESIAN_POINT('Ctrl Pts',(0.118254395260805,0.575278831782372,
4.81354677224418));
#17085=CARTESIAN_POINT('Ctrl Pts',(0.133884278389959,0.588213103126366,
4.81));
#17086=CARTESIAN_POINT('',(-0.21,0.75,4.81));
#17087=CARTESIAN_POINT('Origin',(0.,0.75,4.81));
#17088=CARTESIAN_POINT('',(-0.21,0.75,5.29976849370594));
#17089=CARTESIAN_POINT('',(-0.21,0.75,4.81));
#17090=CARTESIAN_POINT('',(0.21,0.75,5.29976849370594));
#17091=CARTESIAN_POINT('Ctrl Pts',(0.21,0.75,5.29976849370594));
#17092=CARTESIAN_POINT('Ctrl Pts',(0.21,0.723561411869493,5.29976849370594));
#17093=CARTESIAN_POINT('Ctrl Pts',(0.204702922670976,0.695406218745069,
5.30084015664674));
#17094=CARTESIAN_POINT('Ctrl Pts',(0.183251796806354,0.643686554458656,
5.30468313707126));
#17095=CARTESIAN_POINT('Ctrl Pts',(0.167101177357214,0.620116329258865,
5.30739593054622));
#17096=CARTESIAN_POINT('Ctrl Pts',(0.129884533480965,0.582899685382615,
5.31246633289124));
#17097=CARTESIAN_POINT('Ctrl Pts',(0.106313940757289,0.566748389836589,
5.31515738895358));
#17098=CARTESIAN_POINT('Ctrl Pts',(0.0545930033295205,0.545296773430262,
5.31895039220591));
#17099=CARTESIAN_POINT('Ctrl Pts',(0.0264373623835353,0.54,5.32));
#17100=CARTESIAN_POINT('Ctrl Pts',(-0.0264373623835353,0.54,5.32));
#17101=CARTESIAN_POINT('Ctrl Pts',(-0.0545930033295205,0.545296773430262,
5.31895039220591));
#17102=CARTESIAN_POINT('Ctrl Pts',(-0.106313940757289,0.566748389836589,
5.31515738895358));
#17103=CARTESIAN_POINT('Ctrl Pts',(-0.129884533480965,0.582899685382615,
5.31246633289124));
#17104=CARTESIAN_POINT('Ctrl Pts',(-0.167101177357214,0.620116329258865,
5.30739593054622));
#17105=CARTESIAN_POINT('Ctrl Pts',(-0.183251796806354,0.643686554458656,
5.30468313707126));
#17106=CARTESIAN_POINT('Ctrl Pts',(-0.204702922670976,0.695406218745069,
5.30084015664674));
#17107=CARTESIAN_POINT('Ctrl Pts',(-0.21,0.723561411869493,5.29976849370594));
#17108=CARTESIAN_POINT('Ctrl Pts',(-0.21,0.75,5.29976849370594));
#17109=CARTESIAN_POINT('Ctrl Pts',(-0.21,0.75,5.29976849370594));
#17110=CARTESIAN_POINT('Ctrl Pts',(-0.21,0.776438588130507,5.29976849370594));
#17111=CARTESIAN_POINT('Ctrl Pts',(-0.204702922670976,0.804593781254931,
5.30084015664674));
#17112=CARTESIAN_POINT('Ctrl Pts',(-0.183251796806354,0.856313445541343,
5.30468313707126));
#17113=CARTESIAN_POINT('Ctrl Pts',(-0.167101177357215,0.879883670741135,
5.30739593054622));
#17114=CARTESIAN_POINT('Ctrl Pts',(-0.129884533480965,0.917100314617385,
5.31246633289124));
#17115=CARTESIAN_POINT('Ctrl Pts',(-0.106313940757289,0.933251610163411,
5.31515738895358));
#17116=CARTESIAN_POINT('Ctrl Pts',(-0.0545930033295205,0.954703226569738,
5.31895039220591));
#17117=CARTESIAN_POINT('Ctrl Pts',(-0.0264373623835353,0.96,5.32));
#17118=CARTESIAN_POINT('Ctrl Pts',(0.0264373623835353,0.96,5.32));
#17119=CARTESIAN_POINT('Ctrl Pts',(0.0545930033295204,0.954703226569738,
5.31895039220591));
#17120=CARTESIAN_POINT('Ctrl Pts',(0.106313940757288,0.933251610163411,
5.31515738895358));
#17121=CARTESIAN_POINT('Ctrl Pts',(0.129884533480965,0.917100314617385,
5.31246633289124));
#17122=CARTESIAN_POINT('Ctrl Pts',(0.167101177357214,0.879883670741136,
5.30739593054622));
#17123=CARTESIAN_POINT('Ctrl Pts',(0.183251796806354,0.856313445541344,
5.30468313707126));
#17124=CARTESIAN_POINT('Ctrl Pts',(0.204702922670976,0.804593781254931,
5.30084015664674));
#17125=CARTESIAN_POINT('Ctrl Pts',(0.21,0.776438588130507,5.29976849370594));
#17126=CARTESIAN_POINT('Ctrl Pts',(0.21,0.75,5.29976849370594));
#17127=CARTESIAN_POINT('',(-0.133884278389959,0.911786896873634,4.81));
#17128=CARTESIAN_POINT('Origin',(0.,0.75,4.81));
#17129=CARTESIAN_POINT('Ctrl Pts',(0.133884278389959,0.911786896873634,
4.81));
#17130=CARTESIAN_POINT('Ctrl Pts',(0.118254395260805,0.924721168217627,
4.81354677224418));
#17131=CARTESIAN_POINT('Ctrl Pts',(0.1001097876823,0.935799316587437,4.81698224789957));
#17132=CARTESIAN_POINT('Ctrl Pts',(0.0548298721325192,0.954638561054429,
4.8230741628997));
#17133=CARTESIAN_POINT('Ctrl Pts',(0.0266020595922903,0.96,4.825));
#17134=CARTESIAN_POINT('Ctrl Pts',(-0.0266020595922903,0.96,4.825));
#17135=CARTESIAN_POINT('Ctrl Pts',(-0.0548298721325192,0.954638561054429,
4.8230741628997));
#17136=CARTESIAN_POINT('Ctrl Pts',(-0.1001097876823,0.935799316587437,4.81698224789957));
#17137=CARTESIAN_POINT('Ctrl Pts',(-0.118254395260804,0.924721168217628,
4.81354677224418));
#17138=CARTESIAN_POINT('Ctrl Pts',(-0.133884278389959,0.911786896873634,
4.81));
#17139=CARTESIAN_POINT('Origin',(0.,0.75,4.81));
#17140=CARTESIAN_POINT('',(-0.133884278389959,0.35,4.81));
#17141=CARTESIAN_POINT('Origin',(0.,0.35,4.22));
#17142=CARTESIAN_POINT('',(-0.605,1.15,4.22));
#17143=CARTESIAN_POINT('Origin',(0.,1.15,4.22));
#17144=CARTESIAN_POINT('',(-0.605,0.35,4.22));
#17145=CARTESIAN_POINT('',(-0.605,0.35,4.22));
#17146=CARTESIAN_POINT('Origin',(0.,0.35,4.22));
#17147=CARTESIAN_POINT('Origin',(0.,0.35,4.22));
#17148=CARTESIAN_POINT('',(-1.1,1.15,4.22));
#17149=CARTESIAN_POINT('Origin',(0.,1.15,4.22));
#17150=CARTESIAN_POINT('',(-1.1,0.35,4.22));
#17151=CARTESIAN_POINT('',(-1.1,0.35,4.22));
#17152=CARTESIAN_POINT('Origin',(0.,0.35,4.22));
#17153=CARTESIAN_POINT('Origin',(0.,1.15,4.22));
#17154=CARTESIAN_POINT('Origin',(0.,0.35,4.22));
#17155=CARTESIAN_POINT('',(0.,0.,0.));
#17156=CARTESIAN_POINT('Origin',(0.,20.85,4.81));
#17157=CARTESIAN_POINT('',(0.133884278389959,20.6882131031264,4.81));
#17158=CARTESIAN_POINT('',(0.133884278389959,21.0117868968736,4.81));
#17159=CARTESIAN_POINT('',(0.133884278389959,20.45,4.81));
#17160=CARTESIAN_POINT('Origin',(0.,20.85,4.81));
#17161=CARTESIAN_POINT('Origin',(0.,20.85,4.81));
#17162=CARTESIAN_POINT('',(-0.133884278389959,20.6882131031264,4.81));
#17163=CARTESIAN_POINT('Ctrl Pts',(-0.133884278389959,20.6882131031264,
4.81));
#17164=CARTESIAN_POINT('Ctrl Pts',(-0.118254395260803,20.6752788317824,
4.81354677224418));
#17165=CARTESIAN_POINT('Ctrl Pts',(-0.100109787682301,20.6642006834126,
4.81698224789957));
#17166=CARTESIAN_POINT('Ctrl Pts',(-0.0548298721325192,20.6453614389456,
4.8230741628997));
#17167=CARTESIAN_POINT('Ctrl Pts',(-0.0266020595922905,20.64,4.825));
#17168=CARTESIAN_POINT('Ctrl Pts',(0.0266020595922904,20.64,4.825));
#17169=CARTESIAN_POINT('Ctrl Pts',(0.0548298721325191,20.6453614389456,
4.8230741628997));
#17170=CARTESIAN_POINT('Ctrl Pts',(0.100109787682301,20.6642006834126,4.81698224789957));
#17171=CARTESIAN_POINT('Ctrl Pts',(0.118254395260803,20.6752788317824,4.81354677224418));
#17172=CARTESIAN_POINT('Ctrl Pts',(0.133884278389958,20.6882131031264,4.81));
#17173=CARTESIAN_POINT('',(-0.21,20.85,4.81));
#17174=CARTESIAN_POINT('Origin',(0.,20.85,4.81));
#17175=CARTESIAN_POINT('',(-0.21,20.85,5.29976849370594));
#17176=CARTESIAN_POINT('',(-0.21,20.85,4.81));
#17177=CARTESIAN_POINT('',(0.21,20.85,5.29976849370594));
#17178=CARTESIAN_POINT('Ctrl Pts',(0.21,20.85,5.29976849370594));
#17179=CARTESIAN_POINT('Ctrl Pts',(0.21,20.8235614118695,5.29976849370594));
#17180=CARTESIAN_POINT('Ctrl Pts',(0.204702922670976,20.7954062187451,5.30084015664674));
#17181=CARTESIAN_POINT('Ctrl Pts',(0.183251796806354,20.7436865544587,5.30468313707126));
#17182=CARTESIAN_POINT('Ctrl Pts',(0.167101177357214,20.7201163292589,5.30739593054622));
#17183=CARTESIAN_POINT('Ctrl Pts',(0.129884533480965,20.6828996853826,5.31246633289124));
#17184=CARTESIAN_POINT('Ctrl Pts',(0.106313940757288,20.6667483898366,5.31515738895358));
#17185=CARTESIAN_POINT('Ctrl Pts',(0.0545930033295199,20.6452967734303,
5.31895039220591));
#17186=CARTESIAN_POINT('Ctrl Pts',(0.0264373623835355,20.64,5.32));
#17187=CARTESIAN_POINT('Ctrl Pts',(-0.0264373623835354,20.64,5.32));
#17188=CARTESIAN_POINT('Ctrl Pts',(-0.0545930033295199,20.6452967734303,
5.31895039220591));
#17189=CARTESIAN_POINT('Ctrl Pts',(-0.106313940757288,20.6667483898366,
5.31515738895358));
#17190=CARTESIAN_POINT('Ctrl Pts',(-0.129884533480965,20.6828996853826,
5.31246633289124));
#17191=CARTESIAN_POINT('Ctrl Pts',(-0.167101177357214,20.7201163292589,
5.30739593054622));
#17192=CARTESIAN_POINT('Ctrl Pts',(-0.183251796806354,20.7436865544587,
5.30468313707126));
#17193=CARTESIAN_POINT('Ctrl Pts',(-0.204702922670976,20.7954062187451,
5.30084015664674));
#17194=CARTESIAN_POINT('Ctrl Pts',(-0.21,20.8235614118695,5.29976849370594));
#17195=CARTESIAN_POINT('Ctrl Pts',(-0.21,20.85,5.29976849370594));
#17196=CARTESIAN_POINT('Ctrl Pts',(-0.21,20.85,5.29976849370594));
#17197=CARTESIAN_POINT('Ctrl Pts',(-0.21,20.8764385881305,5.29976849370594));
#17198=CARTESIAN_POINT('Ctrl Pts',(-0.204702922670976,20.9045937812549,
5.30084015664674));
#17199=CARTESIAN_POINT('Ctrl Pts',(-0.183251796806354,20.9563134455413,
5.30468313707126));
#17200=CARTESIAN_POINT('Ctrl Pts',(-0.167101177357214,20.9798836707411,
5.30739593054622));
#17201=CARTESIAN_POINT('Ctrl Pts',(-0.129884533480965,21.0171003146174,
5.31246633289124));
#17202=CARTESIAN_POINT('Ctrl Pts',(-0.106313940757288,21.0332516101634,
5.31515738895358));
#17203=CARTESIAN_POINT('Ctrl Pts',(-0.0545930033295199,21.0547032265697,
5.31895039220591));
#17204=CARTESIAN_POINT('Ctrl Pts',(-0.0264373623835355,21.06,5.32));
#17205=CARTESIAN_POINT('Ctrl Pts',(0.0264373623835354,21.06,5.32));
#17206=CARTESIAN_POINT('Ctrl Pts',(0.0545930033295199,21.0547032265697,
5.31895039220591));
#17207=CARTESIAN_POINT('Ctrl Pts',(0.106313940757288,21.0332516101634,5.31515738895358));
#17208=CARTESIAN_POINT('Ctrl Pts',(0.129884533480965,21.0171003146174,5.31246633289124));
#17209=CARTESIAN_POINT('Ctrl Pts',(0.167101177357214,20.9798836707411,5.30739593054622));
#17210=CARTESIAN_POINT('Ctrl Pts',(0.183251796806354,20.9563134455413,5.30468313707126));
#17211=CARTESIAN_POINT('Ctrl Pts',(0.204702922670976,20.9045937812549,5.30084015664674));
#17212=CARTESIAN_POINT('Ctrl Pts',(0.21,20.8764385881305,5.29976849370594));
#17213=CARTESIAN_POINT('Ctrl Pts',(0.21,20.85,5.29976849370594));
#17214=CARTESIAN_POINT('',(-0.133884278389959,21.0117868968736,4.81));
#17215=CARTESIAN_POINT('Origin',(0.,20.85,4.81));
#17216=CARTESIAN_POINT('Ctrl Pts',(0.133884278389959,21.0117868968736,4.81));
#17217=CARTESIAN_POINT('Ctrl Pts',(0.118254395260804,21.0247211682176,4.81354677224418));
#17218=CARTESIAN_POINT('Ctrl Pts',(0.100109787682302,21.0357993165874,4.81698224789957));
#17219=CARTESIAN_POINT('Ctrl Pts',(0.0548298721325192,21.0546385610544,
4.8230741628997));
#17220=CARTESIAN_POINT('Ctrl Pts',(0.0266020595922905,21.06,4.825));
#17221=CARTESIAN_POINT('Ctrl Pts',(-0.0266020595922904,21.06,4.825));
#17222=CARTESIAN_POINT('Ctrl Pts',(-0.054829872132519,21.0546385610544,
4.8230741628997));
#17223=CARTESIAN_POINT('Ctrl Pts',(-0.100109787682301,21.0357993165874,
4.81698224789957));
#17224=CARTESIAN_POINT('Ctrl Pts',(-0.118254395260806,21.0247211682176,
4.81354677224418));
#17225=CARTESIAN_POINT('Ctrl Pts',(-0.133884278389962,21.0117868968736,
4.81));
#17226=CARTESIAN_POINT('Origin',(0.,20.85,4.81));
#17227=CARTESIAN_POINT('',(-0.133884278389959,20.45,4.81));
#17228=CARTESIAN_POINT('Origin',(0.,20.45,4.22));
#17229=CARTESIAN_POINT('',(-0.605,21.25,4.22));
#17230=CARTESIAN_POINT('Origin',(0.,21.25,4.22));
#17231=CARTESIAN_POINT('',(-0.605,20.45,4.22));
#17232=CARTESIAN_POINT('',(-0.605,20.45,4.22));
#17233=CARTESIAN_POINT('Origin',(0.,20.45,4.22));
#17234=CARTESIAN_POINT('Origin',(0.,20.45,4.22));
#17235=CARTESIAN_POINT('',(-1.1,21.25,4.22));
#17236=CARTESIAN_POINT('Origin',(0.,21.25,4.22));
#17237=CARTESIAN_POINT('',(-1.1,20.45,4.22));
#17238=CARTESIAN_POINT('',(-1.1,20.45,4.22));
#17239=CARTESIAN_POINT('Origin',(0.,20.45,4.22));
#17240=CARTESIAN_POINT('Origin',(0.,21.25,4.22));
#17241=CARTESIAN_POINT('Origin',(0.,20.45,4.22));
#17242=CARTESIAN_POINT('',(0.,0.,0.));
#17243=CARTESIAN_POINT('Origin',(0.,22.,4.22));
#17244=CARTESIAN_POINT('',(-0.225,22.2,4.22));
#17245=CARTESIAN_POINT('Origin',(0.,22.2,4.22));
#17246=CARTESIAN_POINT('',(-0.225,22.,4.22));
#17247=CARTESIAN_POINT('',(-0.225,22.,4.22));
#17248=CARTESIAN_POINT('Origin',(0.,22.,4.22));
#17249=CARTESIAN_POINT('Origin',(0.,22.,4.22));
#17250=CARTESIAN_POINT('',(-0.8,22.2,4.22));
#17251=CARTESIAN_POINT('Origin',(0.,22.2,4.22));
#17252=CARTESIAN_POINT('',(-0.8,22.,4.22));
#17253=CARTESIAN_POINT('',(-0.8,22.,4.22));
#17254=CARTESIAN_POINT('Origin',(0.,22.,4.22));
#17255=CARTESIAN_POINT('Origin',(0.,22.2,4.22));
#17256=CARTESIAN_POINT('Origin',(0.,22.,4.22));
#17257=CARTESIAN_POINT('',(0.,0.,0.));
#17258=CARTESIAN_POINT('Origin',(0.0577350269189626,0.,-0.1));
#17259=CARTESIAN_POINT('',(0.0577350269189626,0.,-0.1));
#17260=CARTESIAN_POINT('',(0.115470053837925,0.,0.));
#17261=CARTESIAN_POINT('',(0.0934187836487032,0.,-0.0381939203391614));
#17262=CARTESIAN_POINT('',(0.0577350269189626,-0.2,-0.1));
#17263=CARTESIAN_POINT('',(0.0577350269189626,0.,-0.1));
#17264=CARTESIAN_POINT('',(0.115470053837925,-0.2,0.));
#17265=CARTESIAN_POINT('',(0.115470053837925,-0.2,0.));
#17266=CARTESIAN_POINT('',(0.115470053837925,0.,0.));
#17267=CARTESIAN_POINT('Origin',(-0.0577350269189626,0.,-0.1));
#17268=CARTESIAN_POINT('',(-0.0577350269189626,0.,-0.1));
#17269=CARTESIAN_POINT('',(0.0561324865405187,0.,-0.1));
#17270=CARTESIAN_POINT('',(-0.0577350269189626,-0.2,-0.1));
#17271=CARTESIAN_POINT('',(-0.0577350269189626,0.,-0.1));
#17272=CARTESIAN_POINT('',(0.0577350269189626,-0.2,-0.1));
#17273=CARTESIAN_POINT('Origin',(-0.115470053837925,0.,-1.38777878078145E-17));
#17274=CARTESIAN_POINT('',(-0.115470053837925,0.,-1.41410031829988E-17));
#17275=CARTESIAN_POINT('',(-0.0797862971081845,0.,-0.0618060796608387));
#17276=CARTESIAN_POINT('',(-0.115470053837925,-0.2,-1.38777878078145E-17));
#17277=CARTESIAN_POINT('',(-0.115470053837925,0.,-1.41410031829988E-17));
#17278=CARTESIAN_POINT('',(-0.0577350269189626,-0.2,-0.1));
#17279=CARTESIAN_POINT('Origin',(-0.0577350269189626,0.,0.1));
#17280=CARTESIAN_POINT('',(-0.0577350269189626,0.,0.1));
#17281=CARTESIAN_POINT('',(-0.0509187836487033,0.,0.111806079660839));
#17282=CARTESIAN_POINT('',(-0.0577350269189626,-0.2,0.1));
#17283=CARTESIAN_POINT('',(-0.0577350269189626,0.,0.1));
#17284=CARTESIAN_POINT('',(-0.115470053837925,-0.2,-1.41410031829988E-17));
#17285=CARTESIAN_POINT('Origin',(0.0577350269189626,0.,0.1));
#17286=CARTESIAN_POINT('',(0.0577350269189626,0.,0.1));
#17287=CARTESIAN_POINT('',(0.113867513459481,0.,0.1));
#17288=CARTESIAN_POINT('',(0.0577350269189626,-0.2,0.1));
#17289=CARTESIAN_POINT('',(0.0577350269189626,0.,0.1));
#17290=CARTESIAN_POINT('',(-0.0577350269189626,-0.2,0.1));
#17291=CARTESIAN_POINT('Origin',(0.115470053837925,0.,0.));
#17292=CARTESIAN_POINT('',(0.122286297108185,0.,-0.0118060796608386));
#17293=CARTESIAN_POINT('',(0.0577350269189626,-0.2,0.1));
#17294=CARTESIAN_POINT('Origin',(0.,-0.2,0.));
#17295=CARTESIAN_POINT('Origin',(0.17,0.,0.));
#17296=CARTESIAN_POINT('',(-0.17,-8.67361737988404E-18,-2.0818995585505E-17));
#17297=CARTESIAN_POINT('Origin',(0.,0.,0.));
#17298=CARTESIAN_POINT('Origin',(0.,-0.015,0.));
#17299=CARTESIAN_POINT('',(-0.1954,-0.0254,-2.39295984553393E-17));
#17300=CARTESIAN_POINT('Origin',(0.,-0.0254,0.));
#17301=CARTESIAN_POINT('',(-0.185,-0.015,-2.2655965784226E-17));
#17302=CARTESIAN_POINT('Origin',(0.,-0.2775,0.));
#17303=CARTESIAN_POINT('',(-0.1954,-0.5296,2.39295984553393E-17));
#17304=CARTESIAN_POINT('Origin',(0.,-0.5296,0.));
#17305=CARTESIAN_POINT('',(-0.1954,-0.2775,-2.39295984553393E-17));
#17306=CARTESIAN_POINT('Origin',(0.,-0.5625,0.));
#17307=CARTESIAN_POINT('',(-0.125,-0.6,-1.53080849893419E-17));
#17308=CARTESIAN_POINT('Origin',(0.,-0.6,0.));
#17309=CARTESIAN_POINT('',(-0.1625,-0.5625,-1.99005104861445E-17));
#17310=CARTESIAN_POINT('Origin',(0.,-0.6,0.));
#17311=CARTESIAN_POINT('',(0.,0.,0.));
#17312=CARTESIAN_POINT('',(0.,0.,0.));
#17313=CARTESIAN_POINT('Origin',(0.,-1.525,0.));
#17314=CARTESIAN_POINT('',(0.21,-1.525,0.562049819855856));
#17315=CARTESIAN_POINT('',(-0.21,-1.525,0.562049819855856));
#17316=CARTESIAN_POINT('Ctrl Pts',(0.21,-1.525,0.562049819855856));
#17317=CARTESIAN_POINT('Ctrl Pts',(0.21,-1.49837871751922,0.562049819855856));
#17318=CARTESIAN_POINT('Ctrl Pts',(0.204633348688358,-1.4701551027118,0.564140225270058));
#17319=CARTESIAN_POINT('Ctrl Pts',(0.183136586201564,-1.41849286725608,
0.571480520223595));
#17320=CARTESIAN_POINT('Ctrl Pts',(0.167016776838808,-1.39503192874046,
0.576602928616412));
#17321=CARTESIAN_POINT('Ctrl Pts',(0.129978636309075,-1.35799378821073,
0.586063715219224));
#17322=CARTESIAN_POINT('Ctrl Pts',(0.106513536936886,-1.34186587223919,
0.591045521796147));
#17323=CARTESIAN_POINT('Ctrl Pts',(0.0548356965671431,-1.32036302924048,
0.598057680137));
#17324=CARTESIAN_POINT('Ctrl Pts',(0.0266060994851219,-1.315,0.6));
#17325=CARTESIAN_POINT('Ctrl Pts',(-0.026606099485122,-1.315,0.6));
#17326=CARTESIAN_POINT('Ctrl Pts',(-0.0548356965671431,-1.32036302924048,
0.598057680137));
#17327=CARTESIAN_POINT('Ctrl Pts',(-0.106513536936886,-1.34186587223919,
0.591045521796147));
#17328=CARTESIAN_POINT('Ctrl Pts',(-0.129978636309075,-1.35799378821073,
0.586063715219224));
#17329=CARTESIAN_POINT('Ctrl Pts',(-0.167016776838808,-1.39503192874046,
0.576602928616412));
#17330=CARTESIAN_POINT('Ctrl Pts',(-0.183136586201564,-1.41849286725608,
0.571480520223595));
#17331=CARTESIAN_POINT('Ctrl Pts',(-0.204633348688358,-1.4701551027118,
0.564140225270058));
#17332=CARTESIAN_POINT('Ctrl Pts',(-0.21,-1.49837871751922,0.562049819855856));
#17333=CARTESIAN_POINT('Ctrl Pts',(-0.21,-1.525,0.562049819855856));
#17334=CARTESIAN_POINT('Ctrl Pts',(-0.21,-1.525,0.562049819855856));
#17335=CARTESIAN_POINT('Ctrl Pts',(-0.21,-1.55162128248078,0.562049819855856));
#17336=CARTESIAN_POINT('Ctrl Pts',(-0.204633348688358,-1.5798448972882,
0.564140225270058));
#17337=CARTESIAN_POINT('Ctrl Pts',(-0.183136586201564,-1.63150713274392,
0.571480520223595));
#17338=CARTESIAN_POINT('Ctrl Pts',(-0.167016776838808,-1.65496807125954,
0.576602928616412));
#17339=CARTESIAN_POINT('Ctrl Pts',(-0.129978636309075,-1.69200621178927,
0.586063715219224));
#17340=CARTESIAN_POINT('Ctrl Pts',(-0.106513536936886,-1.70813412776081,
0.591045521796147));
#17341=CARTESIAN_POINT('Ctrl Pts',(-0.0548356965671429,-1.72963697075952,
0.598057680137));
#17342=CARTESIAN_POINT('Ctrl Pts',(-0.026606099485122,-1.735,0.6));
#17343=CARTESIAN_POINT('Ctrl Pts',(0.026606099485122,-1.735,0.6));
#17344=CARTESIAN_POINT('Ctrl Pts',(0.0548356965671429,-1.72963697075952,
0.598057680137));
#17345=CARTESIAN_POINT('Ctrl Pts',(0.106513536936886,-1.70813412776081,
0.591045521796147));
#17346=CARTESIAN_POINT('Ctrl Pts',(0.129978636309075,-1.69200621178927,
0.586063715219224));
#17347=CARTESIAN_POINT('Ctrl Pts',(0.167016776838808,-1.65496807125954,
0.576602928616412));
#17348=CARTESIAN_POINT('Ctrl Pts',(0.183136586201564,-1.63150713274392,
0.571480520223595));
#17349=CARTESIAN_POINT('Ctrl Pts',(0.204633348688358,-1.5798448972882,0.564140225270058));
#17350=CARTESIAN_POINT('Ctrl Pts',(0.21,-1.55162128248078,0.562049819855856));
#17351=CARTESIAN_POINT('Ctrl Pts',(0.21,-1.525,0.562049819855856));
#17352=CARTESIAN_POINT('',(-0.21,-1.525,1.35380944006164));
#17353=CARTESIAN_POINT('',(-0.21,-1.525,0.));
#17354=CARTESIAN_POINT('Ctrl Pts',(-0.21,-1.525,1.35380944006164));
#17355=CARTESIAN_POINT('Ctrl Pts',(-0.21,-1.49858689919462,1.35380944006164));
#17356=CARTESIAN_POINT('Ctrl Pts',(-0.204712795751841,-1.47044219200607,
1.35466231450937));
#17357=CARTESIAN_POINT('Ctrl Pts',(-0.183268700413686,-1.41871515620915,
1.35772968493193));
#17358=CARTESIAN_POINT('Ctrl Pts',(-0.167114046419118,-1.39512919832077,
1.35989844568037));
#17359=CARTESIAN_POINT('Ctrl Pts',(-0.129871156089225,-1.35788630799087,
1.36395907436197));
#17360=CARTESIAN_POINT('Ctrl Pts',(-0.106285045427176,-1.34173137598416,
1.36611666311719));
#17361=CARTESIAN_POINT('Ctrl Pts',(-0.0545574871667227,-1.32028707843824,
1.36915840160825));
#17362=CARTESIAN_POINT('Ctrl Pts',(-0.026412598106597,-1.315,1.37));
#17363=CARTESIAN_POINT('Ctrl Pts',(0.0264125981065971,-1.315,1.37));
#17364=CARTESIAN_POINT('Ctrl Pts',(0.0545574871667228,-1.32028707843824,
1.36915840160825));
#17365=CARTESIAN_POINT('Ctrl Pts',(0.106285045427176,-1.34173137598416,
1.36611666311719));
#17366=CARTESIAN_POINT('Ctrl Pts',(0.129871156089225,-1.35788630799087,
1.36395907436197));
#17367=CARTESIAN_POINT('Ctrl Pts',(0.167114046419118,-1.39512919832077,
1.35989844568037));
#17368=CARTESIAN_POINT('Ctrl Pts',(0.183268700413687,-1.41871515620915,
1.35772968493193));
#17369=CARTESIAN_POINT('Ctrl Pts',(0.204712795751841,-1.47044219200607,
1.35466231450937));
#17370=CARTESIAN_POINT('Ctrl Pts',(0.21,-1.49858689919462,1.35380944006164));
#17371=CARTESIAN_POINT('Ctrl Pts',(0.21,-1.55141310080538,1.35380944006164));
#17372=CARTESIAN_POINT('Ctrl Pts',(0.204712795751841,-1.57955780799393,
1.35466231450937));
#17373=CARTESIAN_POINT('Ctrl Pts',(0.183268700413686,-1.63128484379085,
1.35772968493193));
#17374=CARTESIAN_POINT('Ctrl Pts',(0.167114046419118,-1.65487080167923,
1.35989844568037));
#17375=CARTESIAN_POINT('Ctrl Pts',(0.129871156089225,-1.69211369200913,
1.36395907436197));
#17376=CARTESIAN_POINT('Ctrl Pts',(0.106285045427176,-1.70826862401584,
1.36611666311719));
#17377=CARTESIAN_POINT('Ctrl Pts',(0.0545574871667227,-1.72971292156176,
1.36915840160825));
#17378=CARTESIAN_POINT('Ctrl Pts',(0.0264125981065971,-1.735,1.37));
#17379=CARTESIAN_POINT('Ctrl Pts',(-0.026412598106597,-1.735,1.37));
#17380=CARTESIAN_POINT('Ctrl Pts',(-0.0545574871667227,-1.72971292156176,
1.36915840160825));
#17381=CARTESIAN_POINT('Ctrl Pts',(-0.106285045427176,-1.70826862401584,
1.36611666311719));
#17382=CARTESIAN_POINT('Ctrl Pts',(-0.129871156089225,-1.69211369200912,
1.36395907436197));
#17383=CARTESIAN_POINT('Ctrl Pts',(-0.167114046419118,-1.65487080167923,
1.35989844568037));
#17384=CARTESIAN_POINT('Ctrl Pts',(-0.183268700413686,-1.63128484379085,
1.35772968493193));
#17385=CARTESIAN_POINT('Ctrl Pts',(-0.204712795751841,-1.57955780799393,
1.35466231450937));
#17386=CARTESIAN_POINT('Ctrl Pts',(-0.21,-1.55141310080538,1.35380944006164));
#17387=CARTESIAN_POINT('Ctrl Pts',(-0.21,-1.525,1.35380944006164));
#17388=CARTESIAN_POINT('Origin',(0.,0.,0.));
#17389=CARTESIAN_POINT('',(-0.6,-2.05,7.34788079488412E-17));
#17390=CARTESIAN_POINT('Origin',(0.,-2.05,0.));
#17391=CARTESIAN_POINT('',(-0.6,-1.,-7.34788079488412E-17));
#17392=CARTESIAN_POINT('',(-0.6,0.,7.34788079488412E-17));
#17393=CARTESIAN_POINT('Origin',(0.,-1.,0.));
#17394=CARTESIAN_POINT('Origin',(-0.999913779596035,-0.4,0.936521453771333));
#17395=CARTESIAN_POINT('',(-1.08689407619899,-0.4,0.834003157741947));
#17396=CARTESIAN_POINT('',(-0.999913779596035,-0.4,0.936521453771333));
#17397=CARTESIAN_POINT('',(-1.08689407619899,-0.4,0.834003157741947));
#17398=CARTESIAN_POINT('',(-1.08689407619899,-1.,0.834003157741947));
#17399=CARTESIAN_POINT('',(-1.08689407619899,-0.4,0.834003157741947));
#17400=CARTESIAN_POINT('',(-0.999913779596035,-1.,0.936521453771333));
#17401=CARTESIAN_POINT('',(-1.02165885374678,-1.,0.910891879763986));
#17402=CARTESIAN_POINT('',(-0.999913779596035,-0.4,0.936521453771333));
#17403=CARTESIAN_POINT('Origin',(-0.903303766687095,-0.4,1.0300205362462));
#17404=CARTESIAN_POINT('',(-0.903303766687095,-0.4,1.0300205362462));
#17405=CARTESIAN_POINT('',(-0.999913779596035,-0.4,0.936521453771333));
#17406=CARTESIAN_POINT('',(-0.903303766687095,-1.,1.0300205362462));
#17407=CARTESIAN_POINT('',(-0.92745626991433,-1.,1.00664576562748));
#17408=CARTESIAN_POINT('',(-0.903303766687095,-0.4,1.0300205362462));
#17409=CARTESIAN_POINT('Origin',(-0.79799444470889,-0.4,1.11359995789051));
#17410=CARTESIAN_POINT('',(-0.79799444470889,-0.4,1.11359995789051));
#17411=CARTESIAN_POINT('',(-0.903303766687095,-0.4,1.0300205362462));
#17412=CARTESIAN_POINT('',(-0.79799444470889,-1.,1.11359995789051));
#17413=CARTESIAN_POINT('',(-0.824321775203442,-1.,1.09270510247943));
#17414=CARTESIAN_POINT('',(-0.79799444470889,-0.4,1.11359995789051));
#17415=CARTESIAN_POINT('Origin',(-0.685,-0.4,1.18645480318468));
#17416=CARTESIAN_POINT('',(-0.685,-0.4,1.18645480318468));
#17417=CARTESIAN_POINT('',(-0.79799444470889,-0.4,1.11359995789051));
#17418=CARTESIAN_POINT('',(-0.685,-1.,1.18645480318468));
#17419=CARTESIAN_POINT('',(-0.713248611177222,-1.,1.16824109186114));
#17420=CARTESIAN_POINT('',(-0.685,-0.4,1.18645480318468));
#17421=CARTESIAN_POINT('Origin',(-0.565408630832021,-0.4,1.24788344014201));
#17422=CARTESIAN_POINT('',(-0.565408630832021,-0.4,1.24788344014201));
#17423=CARTESIAN_POINT('',(-0.685,-0.4,1.18645480318468));
#17424=CARTESIAN_POINT('',(-0.565408630832022,-1.,1.24788344014201));
#17425=CARTESIAN_POINT('',(-0.595306473124018,-1.,1.23252628090268));
#17426=CARTESIAN_POINT('',(-0.565408630832021,-0.4,1.24788344014201));
#17427=CARTESIAN_POINT('Origin',(-0.440372067465332,-0.4,1.29729427740829));
#17428=CARTESIAN_POINT('',(-0.440372067465332,-0.4,1.29729427740829));
#17429=CARTESIAN_POINT('',(-0.565408630832021,-0.4,1.24788344014201));
#17430=CARTESIAN_POINT('',(-0.440372067465332,-1.,1.29729427740829));
#17431=CARTESIAN_POINT('',(-0.471631208307004,-1.,1.28494156809172));
#17432=CARTESIAN_POINT('',(-0.440372067465332,-0.4,1.29729427740829));
#17433=CARTESIAN_POINT('Origin',(-0.311094480357092,-0.4,1.33421146160995));
#17434=CARTESIAN_POINT('',(-0.311094480357092,-0.4,1.33421146160995));
#17435=CARTESIAN_POINT('',(-0.440372067465332,-0.4,1.29729427740829));
#17436=CARTESIAN_POINT('',(-0.311094480357092,-1.,1.33421146160995));
#17437=CARTESIAN_POINT('',(-0.343413877134152,-1.,1.32498216555953));
#17438=CARTESIAN_POINT('',(-0.311094480357092,-0.4,1.33421146160995));
#17439=CARTESIAN_POINT('Origin',(-0.178820883341471,-0.4,1.35827946008212));
#17440=CARTESIAN_POINT('',(-0.178820883341471,-0.4,1.35827946008212));
#17441=CARTESIAN_POINT('',(-0.311094480357092,-0.4,1.33421146160995));
#17442=CARTESIAN_POINT('',(-0.178820883341471,-1.,1.35827946008212));
#17443=CARTESIAN_POINT('',(-0.211889282595376,-1.,1.35226246046408));
#17444=CARTESIAN_POINT('',(-0.178820883341471,-0.4,1.35827946008212));
#17445=CARTESIAN_POINT('Origin',(-0.104420953776042,-0.4,0.793155889099048));
#17446=CARTESIAN_POINT('',(-0.104420953776042,-0.4,0.793155889099048));
#17447=CARTESIAN_POINT('',(-0.178820883341471,-0.4,1.35827946008212));
#17448=CARTESIAN_POINT('',(-0.104420953776042,-1.,0.793155889099048));
#17449=CARTESIAN_POINT('',(-0.0522104768880209,-1.,0.396577944549524));
#17450=CARTESIAN_POINT('',(-0.104420953776042,-0.4,0.793155889099048));
#17451=CARTESIAN_POINT('Origin',(-0.181661010427499,-0.4,0.779101583421867));
#17452=CARTESIAN_POINT('',(-0.181661010427499,-0.4,0.779101583421867));
#17453=CARTESIAN_POINT('',(-0.104420953776042,-0.4,0.793155889099048));
#17454=CARTESIAN_POINT('',(-0.181661010427499,-1.,0.779101583421867));
#17455=CARTESIAN_POINT('',(-0.162350996264634,-1.,0.782615159841162));
#17456=CARTESIAN_POINT('',(-0.181661010427499,-0.4,0.779101583421867));
#17457=CARTESIAN_POINT('Origin',(-0.25715157224253,-0.4,0.757544103596084));
#17458=CARTESIAN_POINT('',(-0.25715157224253,-0.4,0.757544103596084));
#17459=CARTESIAN_POINT('',(-0.181661010427499,-0.4,0.779101583421867));
#17460=CARTESIAN_POINT('',(-0.25715157224253,-1.,0.757544103596084));
#17461=CARTESIAN_POINT('',(-0.238278931788772,-1.,0.76293347355253));
#17462=CARTESIAN_POINT('',(-0.25715157224253,-0.4,0.757544103596084));
#17463=CARTESIAN_POINT('Origin',(-0.330165623843516,-0.4,0.72869105993694));
#17464=CARTESIAN_POINT('',(-0.330165623843516,-0.4,0.72869105993694));
#17465=CARTESIAN_POINT('',(-0.25715157224253,-0.4,0.757544103596084));
#17466=CARTESIAN_POINT('',(-0.330165623843516,-1.,0.72869105993694));
#17467=CARTESIAN_POINT('',(-0.311912110943269,-1.,0.735904320851726));
#17468=CARTESIAN_POINT('',(-0.330165623843516,-0.4,0.72869105993694));
#17469=CARTESIAN_POINT('Origin',(-0.4,-0.4,0.692820323027551));
#17470=CARTESIAN_POINT('',(-0.4,-0.4,0.692820323027551));
#17471=CARTESIAN_POINT('',(-0.330165623843516,-0.4,0.72869105993694));
#17472=CARTESIAN_POINT('',(-0.4,-1.,0.692820323027551));
#17473=CARTESIAN_POINT('',(-0.382541405960879,-1.,0.701788007254898));
#17474=CARTESIAN_POINT('',(-0.4,-0.4,0.692820323027551));
#17475=CARTESIAN_POINT('Origin',(-0.465982157494242,-0.4,0.650277347673292));
#17476=CARTESIAN_POINT('',(-0.465982157494242,-0.4,0.650277347673292));
#17477=CARTESIAN_POINT('',(-0.4,-0.4,0.692820323027551));
#17478=CARTESIAN_POINT('',(-0.465982157494242,-1.,0.650277347673292));
#17479=CARTESIAN_POINT('',(-0.449486618120682,-1.,0.660913091511857));
#17480=CARTESIAN_POINT('',(-0.465982157494242,-0.4,0.650277347673292));
#17481=CARTESIAN_POINT('Origin',(-0.527476652080055,-0.4,0.601471845983182));
#17482=CARTESIAN_POINT('',(-0.527476652080055,-0.4,0.601471845983182));
#17483=CARTESIAN_POINT('',(-0.465982157494242,-0.4,0.650277347673292));
#17484=CARTESIAN_POINT('',(-0.527476652080055,-1.,0.601471845983182));
#17485=CARTESIAN_POINT('',(-0.512103028433602,-1.,0.613673221405709));
#17486=CARTESIAN_POINT('',(-0.527476652080055,-0.4,0.601471845983182));
#17487=CARTESIAN_POINT('Origin',(-0.583891258158269,-0.4,0.546873841618297));
#17488=CARTESIAN_POINT('',(-0.583891258158269,-0.4,0.546873841618297));
#17489=CARTESIAN_POINT('',(-0.527476652080055,-0.4,0.601471845983182));
#17490=CARTESIAN_POINT('',(-0.583891258158269,-1.,0.546873841618297));
#17491=CARTESIAN_POINT('',(-0.569787606638716,-1.,0.560523342709518));
#17492=CARTESIAN_POINT('',(-0.583891258158269,-0.4,0.546873841618297));
#17493=CARTESIAN_POINT('Origin',(-0.634682672232988,-0.4,0.487009143206976));
#17494=CARTESIAN_POINT('',(-0.634682672232988,-0.4,0.487009143206976));
#17495=CARTESIAN_POINT('',(-0.583891258158269,-0.4,0.546873841618297));
#17496=CARTESIAN_POINT('',(-0.634682672232988,-1.,0.487009143206976));
#17497=CARTESIAN_POINT('',(-0.621984818714309,-1.,0.501975317809806));
#17498=CARTESIAN_POINT('',(-0.634682672232988,-0.4,0.487009143206976));
#17499=CARTESIAN_POINT('Origin',(-1.08689407619899,-0.4,0.834003157741947));
#17500=CARTESIAN_POINT('',(-0.634682672232988,-0.4,0.487009143206976));
#17501=CARTESIAN_POINT('',(-0.543447038099496,-1.,0.417001578870973));
#17502=CARTESIAN_POINT('Origin',(-0.527275906502258,-0.4,0.913268659668846));
#17503=CARTESIAN_POINT('Origin',(0.,-1.,0.));
#17504=CARTESIAN_POINT('Origin',(0.,-1.,0.));
#17505=CARTESIAN_POINT('Origin',(0.,-1.,0.));
#17506=CARTESIAN_POINT('Origin',(0.,-1.,0.));
#17507=CARTESIAN_POINT('Origin',(0.,-1.,0.));
#17508=CARTESIAN_POINT('Origin',(0.,-1.,0.));
#17509=CARTESIAN_POINT('Origin',(0.,-1.,0.));
#17510=CARTESIAN_POINT('Origin',(0.,-1.,0.));
#17511=CARTESIAN_POINT('Origin',(0.,-1.,0.));
#17512=CARTESIAN_POINT('Origin',(0.,-1.,0.));
#17513=CARTESIAN_POINT('Origin',(0.,-1.,0.));
#17514=CARTESIAN_POINT('Origin',(0.,-1.,0.));
#17515=CARTESIAN_POINT('Origin',(0.,-1.,0.));
#17516=CARTESIAN_POINT('Origin',(0.,-1.,0.));
#17517=CARTESIAN_POINT('Origin',(0.,-1.,0.));
#17518=CARTESIAN_POINT('Origin',(0.,-1.,0.));
#17519=CARTESIAN_POINT('Origin',(0.,-1.,0.));
#17520=CARTESIAN_POINT('',(1.26571495954046,-1.,0.524276302340173));
#17521=CARTESIAN_POINT('Origin',(0.,-1.,0.));
#17522=CARTESIAN_POINT('',(0.739103626009029,-1.,0.306146745892072));
#17523=CARTESIAN_POINT('',(0.632857479770231,-1.,0.262138151170086));
#17524=CARTESIAN_POINT('',(0.765552268585767,-1.,0.23222774180357));
#17525=CARTESIAN_POINT('',(0.745715786653214,-1.,0.287666994869947));
#17526=CARTESIAN_POINT('',(0.784628224322584,-1.,0.156072257612903));
#17527=CARTESIAN_POINT('',(0.770321257519971,-1.,0.213188870755903));
#17528=CARTESIAN_POINT('',(0.796147781337758,-1.,0.0784137122636485));
#17529=CARTESIAN_POINT('',(0.787508113576378,-1.,0.136657621275589));
#17530=CARTESIAN_POINT('',(0.8,-1.,0.));
#17531=CARTESIAN_POINT('',(0.797110836003318,-1.,0.0588102841977364));
#17532=CARTESIAN_POINT('',(0.796147781337758,-1.,-0.0784137122636485));
#17533=CARTESIAN_POINT('',(0.799036945334439,-1.,-0.0196034280659122));
#17534=CARTESIAN_POINT('',(0.784628224322584,-1.,-0.156072257612903));
#17535=CARTESIAN_POINT('',(0.793267892083964,-1.,-0.0978283486009621));
#17536=CARTESIAN_POINT('',(0.765552268585767,-1.,-0.23222774180357));
#17537=CARTESIAN_POINT('',(0.77985923538838,-1.,-0.17511112866057));
#17538=CARTESIAN_POINT('',(0.739103626009029,-1.,-0.306146745892072));
#17539=CARTESIAN_POINT('',(0.758940107941583,-1.,-0.250707492825696));
#17540=CARTESIAN_POINT('',(1.26571495954046,-1.,-0.524276302340173));
#17541=CARTESIAN_POINT('',(0.369551813004515,-1.,-0.153073372946036));
#17542=CARTESIAN_POINT('',(-0.17882088334147,-1.,-1.35827946008212));
#17543=CARTESIAN_POINT('Origin',(0.,-1.,0.));
#17544=CARTESIAN_POINT('',(-0.104420953776041,-1.,-0.793155889099048));
#17545=CARTESIAN_POINT('',(-0.0894104416707352,-1.,-0.67913973004106));
#17546=CARTESIAN_POINT('',(-0.181661010427498,-1.,-0.779101583421867));
#17547=CARTESIAN_POINT('',(-0.123730967938905,-1.,-0.789642312679753));
#17548=CARTESIAN_POINT('',(-0.257151572242529,-1.,-0.757544103596085));
#17549=CARTESIAN_POINT('',(-0.200533650881256,-1.,-0.773712213465422));
#17550=CARTESIAN_POINT('',(-0.330165623843516,-1.,-0.728691059936941));
#17551=CARTESIAN_POINT('',(-0.275405085142776,-1.,-0.750330842681299));
#17552=CARTESIAN_POINT('',(-0.4,-1.,-0.692820323027551));
#17553=CARTESIAN_POINT('',(-0.347624217882637,-1.,-0.719723375709593));
#17554=CARTESIAN_POINT('',(-0.465982157494242,-1.,-0.650277347673292));
#17555=CARTESIAN_POINT('',(-0.41649553937356,-1.,-0.682184579188986));
#17556=CARTESIAN_POINT('',(-0.527476652080055,-1.,-0.601471845983182));
#17557=CARTESIAN_POINT('',(-0.481355781140695,-1.,-0.638075972250765));
#17558=CARTESIAN_POINT('',(-0.583891258158268,-1.,-0.546873841618297));
#17559=CARTESIAN_POINT('',(-0.541580303599609,-1.,-0.587822344891961));
#17560=CARTESIAN_POINT('',(-0.634682672232988,-1.,-0.487009143206977));
#17561=CARTESIAN_POINT('',(-0.596589111676948,-1.,-0.531907667015467));
#17562=CARTESIAN_POINT('',(-1.08689407619899,-1.,-0.834003157741947));
#17563=CARTESIAN_POINT('',(-0.317341336116494,-1.,-0.243504571603488));
#17564=CARTESIAN_POINT('',(-1.37,-1.,-1.67776611483187E-16));
#17565=CARTESIAN_POINT('Origin',(0.,-1.,0.));
#17566=CARTESIAN_POINT('Origin',(0.,-1.,0.));
#17567=CARTESIAN_POINT('Origin',(-0.311094480357091,-0.4,-1.33421146160995));
#17568=CARTESIAN_POINT('',(-0.17882088334147,-0.4,-1.35827946008212));
#17569=CARTESIAN_POINT('',(-0.311094480357091,-0.4,-1.33421146160995));
#17570=CARTESIAN_POINT('',(-0.17882088334147,-0.4,-1.35827946008212));
#17571=CARTESIAN_POINT('',(-0.17882088334147,-0.4,-1.35827946008212));
#17572=CARTESIAN_POINT('',(-0.311094480357091,-1.,-1.33421146160995));
#17573=CARTESIAN_POINT('',(-0.278026081103185,-1.,-1.34022846122799));
#17574=CARTESIAN_POINT('',(-0.311094480357091,-0.4,-1.33421146160995));
#17575=CARTESIAN_POINT('Origin',(-0.440372067465331,-0.4,-1.29729427740829));
#17576=CARTESIAN_POINT('',(-0.440372067465331,-0.4,-1.29729427740829));
#17577=CARTESIAN_POINT('',(-0.311094480357091,-0.4,-1.33421146160995));
#17578=CARTESIAN_POINT('',(-0.440372067465331,-1.,-1.29729427740829));
#17579=CARTESIAN_POINT('',(-0.408052670688271,-1.,-1.30652357345871));
#17580=CARTESIAN_POINT('',(-0.440372067465331,-0.4,-1.29729427740829));
#17581=CARTESIAN_POINT('Origin',(-0.565408630832021,-0.4,-1.24788344014201));
#17582=CARTESIAN_POINT('',(-0.565408630832021,-0.4,-1.24788344014201));
#17583=CARTESIAN_POINT('',(-0.440372067465331,-0.4,-1.29729427740829));
#17584=CARTESIAN_POINT('',(-0.565408630832021,-1.,-1.24788344014201));
#17585=CARTESIAN_POINT('',(-0.534149489990348,-1.,-1.26023614945858));
#17586=CARTESIAN_POINT('',(-0.565408630832021,-0.4,-1.24788344014201));
#17587=CARTESIAN_POINT('Origin',(-0.685,-0.4,-1.18645480318468));
#17588=CARTESIAN_POINT('',(-0.685,-0.4,-1.18645480318468));
#17589=CARTESIAN_POINT('',(-0.565408630832021,-0.4,-1.24788344014201));
#17590=CARTESIAN_POINT('',(-0.685,-1.,-1.18645480318468));
#17591=CARTESIAN_POINT('',(-0.655102157708006,-1.,-1.20181196242401));
#17592=CARTESIAN_POINT('',(-0.685,-0.4,-1.18645480318468));
#17593=CARTESIAN_POINT('Origin',(-0.797994444708889,-0.4,-1.11359995789051));
#17594=CARTESIAN_POINT('',(-0.797994444708889,-0.4,-1.11359995789051));
#17595=CARTESIAN_POINT('',(-0.685,-0.4,-1.18645480318468));
#17596=CARTESIAN_POINT('',(-0.797994444708889,-1.,-1.11359995789051));
#17597=CARTESIAN_POINT('',(-0.769745833531665,-1.,-1.13181366921406));
#17598=CARTESIAN_POINT('',(-0.797994444708889,-0.4,-1.11359995789051));
#17599=CARTESIAN_POINT('Origin',(-0.903303766687094,-0.4,-1.0300205362462));
#17600=CARTESIAN_POINT('',(-0.903303766687094,-0.4,-1.0300205362462));
#17601=CARTESIAN_POINT('',(-0.797994444708889,-0.4,-1.11359995789051));
#17602=CARTESIAN_POINT('',(-0.903303766687094,-1.,-1.0300205362462));
#17603=CARTESIAN_POINT('',(-0.876976436192543,-1.,-1.05091539165728));
#17604=CARTESIAN_POINT('',(-0.903303766687094,-0.4,-1.0300205362462));
#17605=CARTESIAN_POINT('Origin',(-0.999913779596035,-0.4,-0.936521453771334));
#17606=CARTESIAN_POINT('',(-0.999913779596035,-0.4,-0.936521453771334));
#17607=CARTESIAN_POINT('',(-0.903303766687094,-0.4,-1.0300205362462));
#17608=CARTESIAN_POINT('',(-0.999913779596034,-1.,-0.936521453771334));
#17609=CARTESIAN_POINT('',(-0.9757612763688,-1.,-0.95989622439005));
#17610=CARTESIAN_POINT('',(-0.999913779596035,-0.4,-0.936521453771334));
#17611=CARTESIAN_POINT('Origin',(-1.08689407619899,-0.4,-0.834003157741947));
#17612=CARTESIAN_POINT('',(-1.08689407619899,-0.4,-0.834003157741947));
#17613=CARTESIAN_POINT('',(-0.999913779596035,-0.4,-0.936521453771334));
#17614=CARTESIAN_POINT('',(-1.06514900204825,-1.,-0.859632731749293));
#17615=CARTESIAN_POINT('',(-1.08689407619899,-0.4,-0.834003157741947));
#17616=CARTESIAN_POINT('Origin',(-0.634682672232988,-0.4,-0.487009143206977));
#17617=CARTESIAN_POINT('',(-0.634682672232988,-0.4,-0.487009143206977));
#17618=CARTESIAN_POINT('',(-1.08689407619899,-0.4,-0.834003157741947));
#17619=CARTESIAN_POINT('',(-0.634682672232988,-0.4,-0.487009143206977));
#17620=CARTESIAN_POINT('Origin',(-0.583891258158268,-0.4,-0.546873841618297));
#17621=CARTESIAN_POINT('',(-0.583891258158268,-0.4,-0.546873841618297));
#17622=CARTESIAN_POINT('',(-0.634682672232988,-0.4,-0.487009143206977));
#17623=CARTESIAN_POINT('',(-0.583891258158268,-0.4,-0.546873841618297));
#17624=CARTESIAN_POINT('Origin',(-0.527476652080055,-0.4,-0.601471845983182));
#17625=CARTESIAN_POINT('',(-0.527476652080055,-0.4,-0.601471845983182));
#17626=CARTESIAN_POINT('',(-0.583891258158268,-0.4,-0.546873841618297));
#17627=CARTESIAN_POINT('',(-0.527476652080055,-0.4,-0.601471845983182));
#17628=CARTESIAN_POINT('Origin',(-0.465982157494242,-0.4,-0.650277347673292));
#17629=CARTESIAN_POINT('',(-0.465982157494242,-0.4,-0.650277347673292));
#17630=CARTESIAN_POINT('',(-0.527476652080055,-0.4,-0.601471845983182));
#17631=CARTESIAN_POINT('',(-0.465982157494242,-0.4,-0.650277347673292));
#17632=CARTESIAN_POINT('Origin',(-0.4,-0.4,-0.692820323027551));
#17633=CARTESIAN_POINT('',(-0.4,-0.4,-0.692820323027551));
#17634=CARTESIAN_POINT('',(-0.465982157494242,-0.4,-0.650277347673292));
#17635=CARTESIAN_POINT('',(-0.4,-0.4,-0.692820323027551));
#17636=CARTESIAN_POINT('Origin',(-0.330165623843516,-0.4,-0.728691059936941));
#17637=CARTESIAN_POINT('',(-0.330165623843516,-0.4,-0.728691059936941));
#17638=CARTESIAN_POINT('',(-0.4,-0.4,-0.692820323027551));
#17639=CARTESIAN_POINT('',(-0.330165623843516,-0.4,-0.728691059936941));
#17640=CARTESIAN_POINT('Origin',(-0.257151572242529,-0.4,-0.757544103596085));
#17641=CARTESIAN_POINT('',(-0.257151572242529,-0.4,-0.757544103596085));
#17642=CARTESIAN_POINT('',(-0.330165623843516,-0.4,-0.728691059936941));
#17643=CARTESIAN_POINT('',(-0.257151572242529,-0.4,-0.757544103596085));
#17644=CARTESIAN_POINT('Origin',(-0.181661010427498,-0.4,-0.779101583421867));
#17645=CARTESIAN_POINT('',(-0.181661010427498,-0.4,-0.779101583421867));
#17646=CARTESIAN_POINT('',(-0.257151572242529,-0.4,-0.757544103596085));
#17647=CARTESIAN_POINT('',(-0.181661010427498,-0.4,-0.779101583421867));
#17648=CARTESIAN_POINT('Origin',(-0.104420953776041,-0.4,-0.793155889099048));
#17649=CARTESIAN_POINT('',(-0.104420953776041,-0.4,-0.793155889099048));
#17650=CARTESIAN_POINT('',(-0.181661010427498,-0.4,-0.779101583421867));
#17651=CARTESIAN_POINT('',(-0.104420953776041,-0.4,-0.793155889099048));
#17652=CARTESIAN_POINT('Origin',(-0.17882088334147,-0.4,-1.35827946008212));
#17653=CARTESIAN_POINT('',(-0.104420953776041,-0.4,-0.793155889099048));
#17654=CARTESIAN_POINT('Origin',(-0.527275906502257,-0.4,-0.913268659668847));
#17655=CARTESIAN_POINT('Origin',(0.,-1.,0.));
#17656=CARTESIAN_POINT('Origin',(0.,-1.,0.));
#17657=CARTESIAN_POINT('Origin',(0.,-1.,0.));
#17658=CARTESIAN_POINT('Origin',(0.,-1.,0.));
#17659=CARTESIAN_POINT('Origin',(0.,-1.,0.));
#17660=CARTESIAN_POINT('Origin',(0.,-1.,0.));
#17661=CARTESIAN_POINT('Origin',(0.,-1.,0.));
#17662=CARTESIAN_POINT('Origin',(0.,-1.,0.));
#17663=CARTESIAN_POINT('Origin',(0.,-1.,0.));
#17664=CARTESIAN_POINT('Origin',(0.,-1.,0.));
#17665=CARTESIAN_POINT('Origin',(0.,-1.,0.));
#17666=CARTESIAN_POINT('Origin',(0.,-1.,0.));
#17667=CARTESIAN_POINT('Origin',(0.,-1.,0.));
#17668=CARTESIAN_POINT('Origin',(0.,-1.,0.));
#17669=CARTESIAN_POINT('Origin',(0.,-1.,0.));
#17670=CARTESIAN_POINT('Origin',(0.,-1.,0.));
#17671=CARTESIAN_POINT('Origin',(1.31100825995313,-0.4,0.397690007838613));
#17672=CARTESIAN_POINT('',(1.26571495954046,-0.4,0.524276302340173));
#17673=CARTESIAN_POINT('',(1.31100825995313,-0.4,0.397690007838613));
#17674=CARTESIAN_POINT('',(1.26571495954046,-0.4,0.524276302340173));
#17675=CARTESIAN_POINT('',(1.26571495954046,-0.4,0.524276302340173));
#17676=CARTESIAN_POINT('',(1.31100825995313,-1.,0.397690007838613));
#17677=CARTESIAN_POINT('',(1.29968493484996,-1.,0.429336581464004));
#17678=CARTESIAN_POINT('',(1.31100825995313,-0.4,0.397690007838613));
#17679=CARTESIAN_POINT('Origin',(1.34367583415243,-0.4,0.267273741162096));
#17680=CARTESIAN_POINT('',(1.34367583415243,-0.4,0.267273741162096));
#17681=CARTESIAN_POINT('',(1.31100825995313,-0.4,0.397690007838613));
#17682=CARTESIAN_POINT('',(1.34367583415243,-1.,0.267273741162096));
#17683=CARTESIAN_POINT('',(1.3355089406026,-1.,0.299877807831226));
#17684=CARTESIAN_POINT('',(1.34367583415243,-0.4,0.267273741162096));
#17685=CARTESIAN_POINT('Origin',(1.36340307554091,-0.4,0.134283482251498));
#17686=CARTESIAN_POINT('',(1.36340307554091,-0.4,0.134283482251498));
#17687=CARTESIAN_POINT('',(1.34367583415243,-0.4,0.267273741162096));
#17688=CARTESIAN_POINT('',(1.36340307554091,-1.,0.134283482251498));
#17689=CARTESIAN_POINT('',(1.35847126519379,-1.,0.167531046979148));
#17690=CARTESIAN_POINT('',(1.36340307554091,-0.4,0.134283482251498));
#17691=CARTESIAN_POINT('Origin',(1.37,-0.4,0.));
#17692=CARTESIAN_POINT('',(1.37,-0.4,0.));
#17693=CARTESIAN_POINT('',(1.36340307554091,-0.4,0.134283482251498));
#17694=CARTESIAN_POINT('',(1.37,-1.,0.));
#17695=CARTESIAN_POINT('',(1.36835076888523,-1.,0.0335708705628731));
#17696=CARTESIAN_POINT('',(1.37,-0.4,0.));
#17697=CARTESIAN_POINT('Origin',(1.36340307554091,-0.4,-0.134283482251498));
#17698=CARTESIAN_POINT('',(1.36340307554091,-0.4,-0.134283482251498));
#17699=CARTESIAN_POINT('',(1.37,-0.4,0.));
#17700=CARTESIAN_POINT('',(1.36340307554091,-1.,-0.134283482251498));
#17701=CARTESIAN_POINT('',(1.36505230665568,-1.,-0.100712611688622));
#17702=CARTESIAN_POINT('',(1.36340307554091,-0.4,-0.134283482251498));
#17703=CARTESIAN_POINT('Origin',(1.34367583415243,-0.4,-0.267273741162096));
#17704=CARTESIAN_POINT('',(1.34367583415243,-0.4,-0.267273741162096));
#17705=CARTESIAN_POINT('',(1.36340307554091,-0.4,-0.134283482251498));
#17706=CARTESIAN_POINT('',(1.34367583415243,-1.,-0.267273741162096));
#17707=CARTESIAN_POINT('',(1.34860764449955,-1.,-0.234026176434447));
#17708=CARTESIAN_POINT('',(1.34367583415243,-0.4,-0.267273741162096));
#17709=CARTESIAN_POINT('Origin',(1.31100825995313,-0.4,-0.397690007838613));
#17710=CARTESIAN_POINT('',(1.31100825995313,-0.4,-0.397690007838613));
#17711=CARTESIAN_POINT('',(1.34367583415243,-0.4,-0.267273741162096));
#17712=CARTESIAN_POINT('',(1.31100825995313,-1.,-0.397690007838613));
#17713=CARTESIAN_POINT('',(1.31917515350295,-1.,-0.365085941169485));
#17714=CARTESIAN_POINT('',(1.31100825995313,-0.4,-0.397690007838613));
#17715=CARTESIAN_POINT('Origin',(1.26571495954046,-0.4,-0.524276302340173));
#17716=CARTESIAN_POINT('',(1.26571495954046,-0.4,-0.524276302340173));
#17717=CARTESIAN_POINT('',(1.31100825995313,-0.4,-0.397690007838613));
#17718=CARTESIAN_POINT('',(1.27703828464363,-1.,-0.492629728714784));
#17719=CARTESIAN_POINT('',(1.26571495954046,-0.4,-0.524276302340173));
#17720=CARTESIAN_POINT('Origin',(0.739103626009029,-0.4,-0.306146745892072));
#17721=CARTESIAN_POINT('',(0.739103626009029,-0.4,-0.306146745892072));
#17722=CARTESIAN_POINT('',(1.26571495954046,-0.4,-0.524276302340173));
#17723=CARTESIAN_POINT('',(0.739103626009029,-0.4,-0.306146745892072));
#17724=CARTESIAN_POINT('Origin',(0.765552268585767,-0.4,-0.23222774180357));
#17725=CARTESIAN_POINT('',(0.765552268585767,-0.4,-0.23222774180357));
#17726=CARTESIAN_POINT('',(0.739103626009029,-0.4,-0.306146745892072));
#17727=CARTESIAN_POINT('',(0.765552268585767,-0.4,-0.23222774180357));
#17728=CARTESIAN_POINT('Origin',(0.784628224322584,-0.4,-0.156072257612903));
#17729=CARTESIAN_POINT('',(0.784628224322584,-0.4,-0.156072257612903));
#17730=CARTESIAN_POINT('',(0.765552268585767,-0.4,-0.23222774180357));
#17731=CARTESIAN_POINT('',(0.784628224322584,-0.4,-0.156072257612903));
#17732=CARTESIAN_POINT('Origin',(0.796147781337758,-0.4,-0.0784137122636485));
#17733=CARTESIAN_POINT('',(0.796147781337758,-0.4,-0.0784137122636485));
#17734=CARTESIAN_POINT('',(0.784628224322584,-0.4,-0.156072257612903));
#17735=CARTESIAN_POINT('',(0.796147781337758,-0.4,-0.0784137122636485));
#17736=CARTESIAN_POINT('Origin',(0.8,-0.4,0.));
#17737=CARTESIAN_POINT('',(0.8,-0.4,0.));
#17738=CARTESIAN_POINT('',(0.796147781337758,-0.4,-0.0784137122636485));
#17739=CARTESIAN_POINT('',(0.8,-0.4,0.));
#17740=CARTESIAN_POINT('Origin',(0.796147781337758,-0.4,0.0784137122636485));
#17741=CARTESIAN_POINT('',(0.796147781337758,-0.4,0.0784137122636485));
#17742=CARTESIAN_POINT('',(0.8,-0.4,0.));
#17743=CARTESIAN_POINT('',(0.796147781337758,-0.4,0.0784137122636485));
#17744=CARTESIAN_POINT('Origin',(0.784628224322584,-0.4,0.156072257612903));
#17745=CARTESIAN_POINT('',(0.784628224322584,-0.4,0.156072257612903));
#17746=CARTESIAN_POINT('',(0.796147781337758,-0.4,0.0784137122636485));
#17747=CARTESIAN_POINT('',(0.784628224322584,-0.4,0.156072257612903));
#17748=CARTESIAN_POINT('Origin',(0.765552268585767,-0.4,0.23222774180357));
#17749=CARTESIAN_POINT('',(0.765552268585767,-0.4,0.23222774180357));
#17750=CARTESIAN_POINT('',(0.784628224322584,-0.4,0.156072257612903));
#17751=CARTESIAN_POINT('',(0.765552268585767,-0.4,0.23222774180357));
#17752=CARTESIAN_POINT('Origin',(0.739103626009029,-0.4,0.306146745892072));
#17753=CARTESIAN_POINT('',(0.739103626009029,-0.4,0.306146745892072));
#17754=CARTESIAN_POINT('',(0.765552268585767,-0.4,0.23222774180357));
#17755=CARTESIAN_POINT('',(0.739103626009029,-0.4,0.306146745892072));
#17756=CARTESIAN_POINT('Origin',(1.26571495954046,-0.4,0.524276302340173));
#17757=CARTESIAN_POINT('',(0.739103626009029,-0.4,0.306146745892072));
#17758=CARTESIAN_POINT('Origin',(1.05455181300451,-0.4,0.));
#17759=CARTESIAN_POINT('Origin',(0.,-1.,0.));
#17760=CARTESIAN_POINT('Origin',(0.,-1.,0.));
#17761=CARTESIAN_POINT('Origin',(0.,-1.,0.));
#17762=CARTESIAN_POINT('Origin',(0.,-1.,0.));
#17763=CARTESIAN_POINT('Origin',(0.,-1.,0.));
#17764=CARTESIAN_POINT('Origin',(0.,-1.,0.));
#17765=CARTESIAN_POINT('Origin',(0.,-1.,0.));
#17766=CARTESIAN_POINT('Origin',(0.,-1.,0.));
#17767=CARTESIAN_POINT('Origin',(0.,-1.,0.));
#17768=CARTESIAN_POINT('Origin',(0.,-1.,0.));
#17769=CARTESIAN_POINT('Origin',(0.,-1.,0.));
#17770=CARTESIAN_POINT('Origin',(0.,-1.,0.));
#17771=CARTESIAN_POINT('Origin',(0.,-1.,0.));
#17772=CARTESIAN_POINT('Origin',(0.,-1.,0.));
#17773=CARTESIAN_POINT('Origin',(0.,-1.,0.));
#17774=CARTESIAN_POINT('Origin',(0.,-1.,0.));
#17775=CARTESIAN_POINT('Origin',(0.,-1.,0.));
#17776=CARTESIAN_POINT('',(-1.37,-2.05,1.67776611483187E-16));
#17777=CARTESIAN_POINT('Origin',(0.,-2.05,0.));
#17778=CARTESIAN_POINT('',(-1.37,-1.,-1.67776611483187E-16));
#17779=CARTESIAN_POINT('Origin',(0.,-2.05,0.));
#17780=CARTESIAN_POINT('',(0.,0.,0.));
#17781=CARTESIAN_POINT('Origin',(0.,1.525,0.));
#17782=CARTESIAN_POINT('',(0.591749422187638,1.525,0.0991595751331958));
#17783=CARTESIAN_POINT('',(0.381749422187638,1.525,0.46289024472266));
#17784=CARTESIAN_POINT('Ctrl Pts',(0.591749422187639,1.525,0.0991595751331958));
#17785=CARTESIAN_POINT('Ctrl Pts',(0.591749422187639,1.55162128248078,0.0991595751331958));
#17786=CARTESIAN_POINT('Ctrl Pts',(0.590876440724725,1.5798448972882,0.104852434209432));
#17787=CARTESIAN_POINT('Ctrl Pts',(0.586484941382362,1.63150713274392,0.127139324098885));
#17788=CARTESIAN_POINT('Ctrl Pts',(0.582861172497722,1.65496807125954,0.143660692707601));
#17789=CARTESIAN_POINT('Ctrl Pts',(0.572535383770674,1.69200621178927,0.180467056616695));
#17790=CARTESIAN_POINT('Ctrl Pts',(0.565117205136936,1.70813412776081,0.203279332063799));
#17791=CARTESIAN_POINT('Ctrl Pts',(0.545350992210601,1.72963697075952,0.251539733807139));
#17792=CARTESIAN_POINT('Ctrl Pts',(0.532918292013224,1.735,0.276958441950268));
#17793=CARTESIAN_POINT('Ctrl Pts',(0.506312192528102,1.735,0.323041558049732));
#17794=CARTESIAN_POINT('Ctrl Pts',(0.490515295643458,1.72963697075952,0.346517946329861));
#17795=CARTESIAN_POINT('Ctrl Pts',(0.45860366820005,1.70813412776081,0.387766189732349));
#17796=CARTESIAN_POINT('Ctrl Pts',(0.442556747461599,1.69200621178927,0.40559665860253));
#17797=CARTESIAN_POINT('Ctrl Pts',(0.415844395658913,1.65496807125954,0.43294223590881));
#17798=CARTESIAN_POINT('Ctrl Pts',(0.403348355180798,1.63150713274392,0.44434119612471));
#17799=CARTESIAN_POINT('Ctrl Pts',(0.386243092036367,1.5798448972882,0.459287791060626));
#17800=CARTESIAN_POINT('Ctrl Pts',(0.381749422187638,1.55162128248078,0.46289024472266));
#17801=CARTESIAN_POINT('Ctrl Pts',(0.381749422187638,1.525,0.46289024472266));
#17802=CARTESIAN_POINT('Ctrl Pts',(0.381749422187638,1.525,0.46289024472266));
#17803=CARTESIAN_POINT('Ctrl Pts',(0.381749422187638,1.49837871751922,0.46289024472266));
#17804=CARTESIAN_POINT('Ctrl Pts',(0.386243092036367,1.4701551027118,0.459287791060626));
#17805=CARTESIAN_POINT('Ctrl Pts',(0.403348355180798,1.41849286725608,0.44434119612471));
#17806=CARTESIAN_POINT('Ctrl Pts',(0.415844395658914,1.39503192874046,0.43294223590881));
#17807=CARTESIAN_POINT('Ctrl Pts',(0.442556747461599,1.35799378821073,0.40559665860253));
#17808=CARTESIAN_POINT('Ctrl Pts',(0.45860366820005,1.34186587223919,0.387766189732349));
#17809=CARTESIAN_POINT('Ctrl Pts',(0.490515295643458,1.32036302924048,0.346517946329861));
#17810=CARTESIAN_POINT('Ctrl Pts',(0.506312192528102,1.315,0.323041558049732));
#17811=CARTESIAN_POINT('Ctrl Pts',(0.532918292013224,1.315,0.276958441950268));
#17812=CARTESIAN_POINT('Ctrl Pts',(0.545350992210601,1.32036302924048,0.251539733807139));
#17813=CARTESIAN_POINT('Ctrl Pts',(0.565117205136936,1.34186587223919,0.203279332063799));
#17814=CARTESIAN_POINT('Ctrl Pts',(0.572535383770674,1.35799378821073,0.180467056616695));
#17815=CARTESIAN_POINT('Ctrl Pts',(0.582861172497722,1.39503192874046,0.143660692707601));
#17816=CARTESIAN_POINT('Ctrl Pts',(0.586484941382362,1.41849286725608,0.127139324098885));
#17817=CARTESIAN_POINT('Ctrl Pts',(0.590876440724725,1.47015510271179,0.104852434209432));
#17818=CARTESIAN_POINT('Ctrl Pts',(0.591749422187638,1.49837871751922,0.0991595751331958));
#17819=CARTESIAN_POINT('Ctrl Pts',(0.591749422187638,1.525,0.0991595751331958));
#17820=CARTESIAN_POINT('',(1.06743336697656,1.525,0.85877005482555));
#17821=CARTESIAN_POINT('',(-0.105,1.525,0.181865334794732));
#17822=CARTESIAN_POINT('',(1.27743336697656,1.525,0.495039385236086));
#17823=CARTESIAN_POINT('Ctrl Pts',(1.27743336697656,1.525,0.495039385236086));
#17824=CARTESIAN_POINT('Ctrl Pts',(1.27743336697656,1.49858689919462,0.495039385236086));
#17825=CARTESIAN_POINT('Ctrl Pts',(1.27552837579046,1.47044219200607,0.500044675653854));
#17826=CARTESIAN_POINT('Ctrl Pts',(1.26746274883014,1.41871515620915,0.520149492189153));
#17827=CARTESIAN_POINT('Ctrl Pts',(1.26126362373573,1.39512919832077,0.535224213312019));
#17828=CARTESIAN_POINT('Ctrl Pts',(1.24615878616438,1.35788630799087,0.56950781678886));
#17829=CARTESIAN_POINT('Ctrl Pts',(1.23623425750631,1.34173137598416,0.591012782176279));
#17830=CARTESIAN_POINT('Ctrl Pts',(1.213004701181,1.32028707843824,0.6373310309511));
#17831=CARTESIAN_POINT('Ctrl Pts',(1.19966110223798,1.315,0.662126019059738));
#17832=CARTESIAN_POINT('Ctrl Pts',(1.17324850413138,1.315,0.707873980940262));
#17833=CARTESIAN_POINT('Ctrl Pts',(1.15844721401428,1.32028707843824,0.731827370657151));
#17834=CARTESIAN_POINT('Ctrl Pts',(1.12994921207913,1.34173137598416,0.775103880940915));
#17835=CARTESIAN_POINT('Ctrl Pts',(1.11628763007516,1.35788630799087,0.794451257573106));
#17836=CARTESIAN_POINT('Ctrl Pts',(1.09414957731662,1.39512919832077,0.824674232368354));
#17837=CARTESIAN_POINT('Ctrl Pts',(1.08419404841645,1.41871515620915,0.837580192742778));
#17838=CARTESIAN_POINT('Ctrl Pts',(1.07081558003862,1.47044219200607,0.854617638855513));
#17839=CARTESIAN_POINT('Ctrl Pts',(1.06743336697656,1.49858689919462,0.85877005482555));
#17840=CARTESIAN_POINT('Ctrl Pts',(1.06743336697656,1.525,0.85877005482555));
#17841=CARTESIAN_POINT('Ctrl Pts',(1.06743336697656,1.525,0.85877005482555));
#17842=CARTESIAN_POINT('Ctrl Pts',(1.06743336697656,1.55141310080538,0.85877005482555));
#17843=CARTESIAN_POINT('Ctrl Pts',(1.07081558003862,1.57955780799393,0.854617638855513));
#17844=CARTESIAN_POINT('Ctrl Pts',(1.08419404841645,1.63128484379085,0.837580192742778));
#17845=CARTESIAN_POINT('Ctrl Pts',(1.09414957731662,1.65487080167923,0.824674232368354));
#17846=CARTESIAN_POINT('Ctrl Pts',(1.11628763007516,1.69211369200913,0.794451257573106));
#17847=CARTESIAN_POINT('Ctrl Pts',(1.12994921207913,1.70826862401584,0.775103880940915));
#17848=CARTESIAN_POINT('Ctrl Pts',(1.15844721401428,1.72971292156176,0.731827370657151));
#17849=CARTESIAN_POINT('Ctrl Pts',(1.17324850413138,1.735,0.707873980940262));
#17850=CARTESIAN_POINT('Ctrl Pts',(1.19966110223798,1.735,0.662126019059738));
#17851=CARTESIAN_POINT('Ctrl Pts',(1.213004701181,1.72971292156176,0.6373310309511));
#17852=CARTESIAN_POINT('Ctrl Pts',(1.23623425750631,1.70826862401584,0.591012782176279));
#17853=CARTESIAN_POINT('Ctrl Pts',(1.24615878616438,1.69211369200913,0.569507816788861));
#17854=CARTESIAN_POINT('Ctrl Pts',(1.26126362373573,1.65487080167923,0.535224213312019));
#17855=CARTESIAN_POINT('Ctrl Pts',(1.26746274883014,1.63128484379085,0.520149492189153));
#17856=CARTESIAN_POINT('Ctrl Pts',(1.27552837579046,1.57955780799392,0.500044675653854));
#17857=CARTESIAN_POINT('Ctrl Pts',(1.27743336697656,1.55141310080538,0.495039385236086));
#17858=CARTESIAN_POINT('Ctrl Pts',(1.27743336697656,1.525,0.495039385236086));
#17859=CARTESIAN_POINT('Origin',(0.,0.,0.));
#17860=CARTESIAN_POINT('',(-0.3,1.,0.519615242270663));
#17861=CARTESIAN_POINT('Origin',(0.,1.,0.));
#17862=CARTESIAN_POINT('',(-0.3,2.05,0.519615242270663));
#17863=CARTESIAN_POINT('',(-0.3,0.,0.519615242270663));
#17864=CARTESIAN_POINT('Origin',(0.,2.05,0.));
#17865=CARTESIAN_POINT('Origin',(0.181661010427498,0.4,0.779101583421867));
#17866=CARTESIAN_POINT('',(0.181661010427498,0.4,0.779101583421867));
#17867=CARTESIAN_POINT('',(0.104420953776041,0.4,0.793155889099048));
#17868=CARTESIAN_POINT('',(0.181661010427498,0.4,0.779101583421867));
#17869=CARTESIAN_POINT('',(0.104420953776041,1.,0.793155889099048));
#17870=CARTESIAN_POINT('',(0.104420953776041,0.4,0.793155889099048));
#17871=CARTESIAN_POINT('',(0.181661010427498,1.,0.779101583421867));
#17872=CARTESIAN_POINT('',(0.162350996264633,1.,0.782615159841162));
#17873=CARTESIAN_POINT('',(0.181661010427498,0.4,0.779101583421867));
#17874=CARTESIAN_POINT('Origin',(0.257151572242529,0.4,0.757544103596085));
#17875=CARTESIAN_POINT('',(0.257151572242529,0.4,0.757544103596085));
#17876=CARTESIAN_POINT('',(0.257151572242529,0.4,0.757544103596085));
#17877=CARTESIAN_POINT('',(0.257151572242529,1.,0.757544103596085));
#17878=CARTESIAN_POINT('',(0.238278931788771,1.,0.76293347355253));
#17879=CARTESIAN_POINT('',(0.257151572242529,0.4,0.757544103596085));
#17880=CARTESIAN_POINT('Origin',(0.330165623843515,0.4,0.728691059936941));
#17881=CARTESIAN_POINT('',(0.330165623843515,0.4,0.728691059936941));
#17882=CARTESIAN_POINT('',(0.330165623843515,0.4,0.728691059936941));
#17883=CARTESIAN_POINT('',(0.330165623843515,1.,0.728691059936941));
#17884=CARTESIAN_POINT('',(0.311912110943269,1.,0.735904320851727));
#17885=CARTESIAN_POINT('',(0.330165623843515,0.4,0.728691059936941));
#17886=CARTESIAN_POINT('Origin',(0.4,0.4,0.692820323027551));
#17887=CARTESIAN_POINT('',(0.4,0.4,0.692820323027551));
#17888=CARTESIAN_POINT('',(0.4,0.4,0.692820323027551));
#17889=CARTESIAN_POINT('',(0.4,1.,0.692820323027551));
#17890=CARTESIAN_POINT('',(0.382541405960878,1.,0.701788007254899));
#17891=CARTESIAN_POINT('',(0.4,0.4,0.692820323027551));
#17892=CARTESIAN_POINT('Origin',(0.465982157494241,0.4,0.650277347673292));
#17893=CARTESIAN_POINT('',(0.465982157494241,0.4,0.650277347673292));
#17894=CARTESIAN_POINT('',(0.465982157494241,0.4,0.650277347673292));
#17895=CARTESIAN_POINT('',(0.465982157494241,1.,0.650277347673292));
#17896=CARTESIAN_POINT('',(0.449486618120681,1.,0.660913091511857));
#17897=CARTESIAN_POINT('',(0.465982157494241,0.4,0.650277347673292));
#17898=CARTESIAN_POINT('Origin',(0.527476652080055,0.4,0.601471845983182));
#17899=CARTESIAN_POINT('',(0.527476652080055,0.4,0.601471845983182));
#17900=CARTESIAN_POINT('',(0.527476652080055,0.4,0.601471845983182));
#17901=CARTESIAN_POINT('',(0.527476652080055,1.,0.601471845983182));
#17902=CARTESIAN_POINT('',(0.512103028433601,1.,0.61367322140571));
#17903=CARTESIAN_POINT('',(0.527476652080055,0.4,0.601471845983182));
#17904=CARTESIAN_POINT('Origin',(0.583891258158268,0.4,0.546873841618297));
#17905=CARTESIAN_POINT('',(0.583891258158268,0.4,0.546873841618297));
#17906=CARTESIAN_POINT('',(0.583891258158268,0.4,0.546873841618297));
#17907=CARTESIAN_POINT('',(0.583891258158268,1.,0.546873841618297));
#17908=CARTESIAN_POINT('',(0.569787606638715,1.,0.560523342709519));
#17909=CARTESIAN_POINT('',(0.583891258158268,0.4,0.546873841618297));
#17910=CARTESIAN_POINT('Origin',(0.634682672232988,0.4,0.487009143206977));
#17911=CARTESIAN_POINT('',(0.634682672232988,0.4,0.487009143206977));
#17912=CARTESIAN_POINT('',(0.634682672232988,0.4,0.487009143206977));
#17913=CARTESIAN_POINT('',(0.634682672232988,1.,0.487009143206977));
#17914=CARTESIAN_POINT('',(0.621984818714308,1.,0.501975317809807));
#17915=CARTESIAN_POINT('',(0.634682672232988,0.4,0.487009143206977));
#17916=CARTESIAN_POINT('Origin',(1.08689407619899,0.4,0.834003157741948));
#17917=CARTESIAN_POINT('',(1.08689407619899,0.4,0.834003157741948));
#17918=CARTESIAN_POINT('',(1.08689407619899,0.4,0.834003157741948));
#17919=CARTESIAN_POINT('',(1.08689407619899,1.,0.834003157741948));
#17920=CARTESIAN_POINT('',(0.543447038099496,1.,0.417001578870974));
#17921=CARTESIAN_POINT('',(1.08689407619899,0.4,0.834003157741948));
#17922=CARTESIAN_POINT('Origin',(0.999913779596034,0.4,0.936521453771334));
#17923=CARTESIAN_POINT('',(0.999913779596034,0.4,0.936521453771334));
#17924=CARTESIAN_POINT('',(0.999913779596034,0.4,0.936521453771334));
#17925=CARTESIAN_POINT('',(0.999913779596034,1.,0.936521453771334));
#17926=CARTESIAN_POINT('',(1.02165885374677,1.,0.910891879763987));
#17927=CARTESIAN_POINT('',(0.999913779596034,0.4,0.936521453771334));
#17928=CARTESIAN_POINT('Origin',(0.903303766687094,0.4,1.0300205362462));
#17929=CARTESIAN_POINT('',(0.903303766687094,0.4,1.0300205362462));
#17930=CARTESIAN_POINT('',(0.903303766687094,0.4,1.0300205362462));
#17931=CARTESIAN_POINT('',(0.903303766687094,1.,1.0300205362462));
#17932=CARTESIAN_POINT('',(0.927456269914329,1.,1.00664576562748));
#17933=CARTESIAN_POINT('',(0.903303766687094,0.4,1.0300205362462));
#17934=CARTESIAN_POINT('Origin',(0.797994444708888,0.4,1.11359995789051));
#17935=CARTESIAN_POINT('',(0.797994444708888,0.4,1.11359995789051));
#17936=CARTESIAN_POINT('',(0.797994444708888,0.4,1.11359995789051));
#17937=CARTESIAN_POINT('',(0.797994444708888,1.,1.11359995789051));
#17938=CARTESIAN_POINT('',(0.82432177520344,1.,1.09270510247943));
#17939=CARTESIAN_POINT('',(0.797994444708888,0.4,1.11359995789051));
#17940=CARTESIAN_POINT('Origin',(0.684999999999999,0.4,1.18645480318468));
#17941=CARTESIAN_POINT('',(0.684999999999999,0.4,1.18645480318468));
#17942=CARTESIAN_POINT('',(0.684999999999999,0.4,1.18645480318468));
#17943=CARTESIAN_POINT('',(0.684999999999999,1.,1.18645480318468));
#17944=CARTESIAN_POINT('',(0.71324861117722,1.,1.16824109186114));
#17945=CARTESIAN_POINT('',(0.684999999999999,0.4,1.18645480318468));
#17946=CARTESIAN_POINT('Origin',(0.56540863083202,0.4,1.24788344014201));
#17947=CARTESIAN_POINT('',(0.56540863083202,0.4,1.24788344014201));
#17948=CARTESIAN_POINT('',(0.56540863083202,0.4,1.24788344014201));
#17949=CARTESIAN_POINT('',(0.56540863083202,1.,1.24788344014201));
#17950=CARTESIAN_POINT('',(0.595306473124016,1.,1.23252628090268));
#17951=CARTESIAN_POINT('',(0.56540863083202,0.4,1.24788344014201));
#17952=CARTESIAN_POINT('Origin',(0.44037206746533,0.4,1.29729427740829));
#17953=CARTESIAN_POINT('',(0.44037206746533,0.4,1.29729427740829));
#17954=CARTESIAN_POINT('',(0.44037206746533,0.4,1.29729427740829));
#17955=CARTESIAN_POINT('',(0.44037206746533,1.,1.29729427740829));
#17956=CARTESIAN_POINT('',(0.471631208307002,1.,1.28494156809172));
#17957=CARTESIAN_POINT('',(0.44037206746533,0.4,1.29729427740829));
#17958=CARTESIAN_POINT('Origin',(0.311094480357091,0.4,1.33421146160995));
#17959=CARTESIAN_POINT('',(0.311094480357091,0.4,1.33421146160995));
#17960=CARTESIAN_POINT('',(0.311094480357091,0.4,1.33421146160995));
#17961=CARTESIAN_POINT('',(0.311094480357091,1.,1.33421146160995));
#17962=CARTESIAN_POINT('',(0.34341387713415,1.,1.32498216555953));
#17963=CARTESIAN_POINT('',(0.311094480357091,0.4,1.33421146160995));
#17964=CARTESIAN_POINT('Origin',(0.17882088334147,0.4,1.35827946008212));
#17965=CARTESIAN_POINT('',(0.17882088334147,0.4,1.35827946008212));
#17966=CARTESIAN_POINT('',(0.17882088334147,0.4,1.35827946008212));
#17967=CARTESIAN_POINT('',(0.17882088334147,1.,1.35827946008212));
#17968=CARTESIAN_POINT('',(0.211889282595374,1.,1.35226246046408));
#17969=CARTESIAN_POINT('',(0.17882088334147,0.4,1.35827946008212));
#17970=CARTESIAN_POINT('Origin',(0.104420953776041,0.4,0.793155889099048));
#17971=CARTESIAN_POINT('',(0.104420953776041,0.4,0.793155889099048));
#17972=CARTESIAN_POINT('',(0.0522104768880204,1.,0.396577944549524));
#17973=CARTESIAN_POINT('Origin',(0.527275906502257,0.4,0.913268659668847));
#17974=CARTESIAN_POINT('Origin',(0.,1.,0.));
#17975=CARTESIAN_POINT('Origin',(0.,1.,0.));
#17976=CARTESIAN_POINT('Origin',(0.,1.,0.));
#17977=CARTESIAN_POINT('Origin',(0.,1.,0.));
#17978=CARTESIAN_POINT('Origin',(0.,1.,0.));
#17979=CARTESIAN_POINT('Origin',(0.,1.,0.));
#17980=CARTESIAN_POINT('Origin',(0.,1.,0.));
#17981=CARTESIAN_POINT('Origin',(0.,1.,0.));
#17982=CARTESIAN_POINT('Origin',(0.,1.,0.));
#17983=CARTESIAN_POINT('Origin',(0.,1.,0.));
#17984=CARTESIAN_POINT('Origin',(0.,1.,0.));
#17985=CARTESIAN_POINT('Origin',(0.,1.,0.));
#17986=CARTESIAN_POINT('Origin',(0.,1.,0.));
#17987=CARTESIAN_POINT('',(-0.685,1.,1.18645480318468));
#17988=CARTESIAN_POINT('Origin',(0.,1.,0.));
#17989=CARTESIAN_POINT('',(-1.26571495954046,1.,0.524276302340173));
#17990=CARTESIAN_POINT('Origin',(0.,1.,0.));
#17991=CARTESIAN_POINT('',(-0.739103626009029,1.,0.306146745892072));
#17992=CARTESIAN_POINT('',(-0.632857479770231,1.,0.262138151170086));
#17993=CARTESIAN_POINT('',(-0.765552268585767,1.,0.23222774180357));
#17994=CARTESIAN_POINT('',(-0.745715786653214,1.,0.287666994869946));
#17995=CARTESIAN_POINT('',(-0.784628224322584,1.,0.156072257612902));
#17996=CARTESIAN_POINT('',(-0.770321257519971,1.,0.213188870755903));
#17997=CARTESIAN_POINT('',(-0.796147781337758,1.,0.0784137122636482));
#17998=CARTESIAN_POINT('',(-0.787508113576378,1.,0.136657621275589));
#17999=CARTESIAN_POINT('',(-0.8,1.,-2.22044604925031E-16));
#18000=CARTESIAN_POINT('',(-0.797110836003318,1.,0.0588102841977362));
#18001=CARTESIAN_POINT('',(-0.796147781337758,1.,-0.0784137122636487));
#18002=CARTESIAN_POINT('',(-0.799036945334439,1.,-0.0196034280659124));
#18003=CARTESIAN_POINT('',(-0.784628224322584,1.,-0.156072257612903));
#18004=CARTESIAN_POINT('',(-0.793267892083964,1.,-0.0978283486009623));
#18005=CARTESIAN_POINT('',(-0.765552268585767,1.,-0.23222774180357));
#18006=CARTESIAN_POINT('',(-0.77985923538838,1.,-0.17511112866057));
#18007=CARTESIAN_POINT('',(-0.739103626009029,1.,-0.306146745892072));
#18008=CARTESIAN_POINT('',(-0.758940107941583,1.,-0.250707492825696));
#18009=CARTESIAN_POINT('',(-1.26571495954046,1.,-0.524276302340173));
#18010=CARTESIAN_POINT('',(-0.369551813004515,1.,-0.153073372946036));
#18011=CARTESIAN_POINT('',(0.178820883341471,1.,-1.35827946008212));
#18012=CARTESIAN_POINT('Origin',(0.,1.,0.));
#18013=CARTESIAN_POINT('',(0.104420953776041,1.,-0.793155889099048));
#18014=CARTESIAN_POINT('',(0.0894104416707354,1.,-0.67913973004106));
#18015=CARTESIAN_POINT('',(0.181661010427499,1.,-0.779101583421867));
#18016=CARTESIAN_POINT('',(0.123730967938906,1.,-0.789642312679753));
#18017=CARTESIAN_POINT('',(0.257151572242529,1.,-0.757544103596084));
#18018=CARTESIAN_POINT('',(0.200533650881256,1.,-0.773712213465421));
#18019=CARTESIAN_POINT('',(0.330165623843516,1.,-0.728691059936941));
#18020=CARTESIAN_POINT('',(0.275405085142776,1.,-0.750330842681299));
#18021=CARTESIAN_POINT('',(0.4,1.,-0.692820323027551));
#18022=CARTESIAN_POINT('',(0.347624217882637,1.,-0.719723375709593));
#18023=CARTESIAN_POINT('',(0.465982157494242,1.,-0.650277347673292));
#18024=CARTESIAN_POINT('',(0.416495539373561,1.,-0.682184579188986));
#18025=CARTESIAN_POINT('',(0.527476652080055,1.,-0.601471845983182));
#18026=CARTESIAN_POINT('',(0.481355781140695,1.,-0.638075972250765));
#18027=CARTESIAN_POINT('',(0.583891258158269,1.,-0.546873841618297));
#18028=CARTESIAN_POINT('',(0.541580303599609,1.,-0.587822344891961));
#18029=CARTESIAN_POINT('',(0.634682672232988,1.,-0.487009143206976));
#18030=CARTESIAN_POINT('',(0.596589111676949,1.,-0.531907667015467));
#18031=CARTESIAN_POINT('',(1.08689407619899,1.,-0.834003157741947));
#18032=CARTESIAN_POINT('',(0.317341336116494,1.,-0.243504571603488));
#18033=CARTESIAN_POINT('Origin',(0.,1.,0.));
#18034=CARTESIAN_POINT('Origin',(0.,1.,0.));
#18035=CARTESIAN_POINT('Origin',(0.,1.,0.));
#18036=CARTESIAN_POINT('Origin',(0.,1.,0.));
#18037=CARTESIAN_POINT('Origin',(0.,1.,0.));
#18038=CARTESIAN_POINT('Origin',(-0.765552268585767,0.4,-0.23222774180357));
#18039=CARTESIAN_POINT('',(-0.765552268585767,0.4,-0.23222774180357));
#18040=CARTESIAN_POINT('',(-0.739103626009029,0.4,-0.306146745892072));
#18041=CARTESIAN_POINT('',(-0.765552268585767,0.4,-0.23222774180357));
#18042=CARTESIAN_POINT('',(-0.739103626009029,0.4,-0.306146745892072));
#18043=CARTESIAN_POINT('',(-0.765552268585767,0.4,-0.23222774180357));
#18044=CARTESIAN_POINT('Origin',(-0.784628224322584,0.4,-0.156072257612903));
#18045=CARTESIAN_POINT('',(-0.784628224322584,0.4,-0.156072257612903));
#18046=CARTESIAN_POINT('',(-0.784628224322584,0.4,-0.156072257612903));
#18047=CARTESIAN_POINT('',(-0.784628224322584,0.4,-0.156072257612903));
#18048=CARTESIAN_POINT('Origin',(-0.796147781337758,0.4,-0.0784137122636487));
#18049=CARTESIAN_POINT('',(-0.796147781337758,0.4,-0.0784137122636487));
#18050=CARTESIAN_POINT('',(-0.796147781337758,0.4,-0.0784137122636487));
#18051=CARTESIAN_POINT('',(-0.796147781337758,0.4,-0.0784137122636487));
#18052=CARTESIAN_POINT('Origin',(-0.8,0.4,-2.22044604925031E-16));
#18053=CARTESIAN_POINT('',(-0.8,0.4,-2.22044604925031E-16));
#18054=CARTESIAN_POINT('',(-0.8,0.4,-2.22044604925031E-16));
#18055=CARTESIAN_POINT('',(-0.8,0.4,-2.22044604925031E-16));
#18056=CARTESIAN_POINT('Origin',(-0.796147781337758,0.4,0.0784137122636482));
#18057=CARTESIAN_POINT('',(-0.796147781337758,0.4,0.0784137122636482));
#18058=CARTESIAN_POINT('',(-0.796147781337758,0.4,0.0784137122636482));
#18059=CARTESIAN_POINT('',(-0.796147781337758,0.4,0.0784137122636482));
#18060=CARTESIAN_POINT('Origin',(-0.784628224322584,0.4,0.156072257612902));
#18061=CARTESIAN_POINT('',(-0.784628224322584,0.4,0.156072257612902));
#18062=CARTESIAN_POINT('',(-0.784628224322584,0.4,0.156072257612902));
#18063=CARTESIAN_POINT('',(-0.784628224322584,0.4,0.156072257612902));
#18064=CARTESIAN_POINT('Origin',(-0.765552268585767,0.4,0.23222774180357));
#18065=CARTESIAN_POINT('',(-0.765552268585767,0.4,0.23222774180357));
#18066=CARTESIAN_POINT('',(-0.765552268585767,0.4,0.23222774180357));
#18067=CARTESIAN_POINT('',(-0.765552268585767,0.4,0.23222774180357));
#18068=CARTESIAN_POINT('Origin',(-0.739103626009029,0.4,0.306146745892072));
#18069=CARTESIAN_POINT('',(-0.739103626009029,0.4,0.306146745892072));
#18070=CARTESIAN_POINT('',(-0.739103626009029,0.4,0.306146745892072));
#18071=CARTESIAN_POINT('',(-0.739103626009029,0.4,0.306146745892072));
#18072=CARTESIAN_POINT('Origin',(-1.26571495954046,0.4,0.524276302340173));
#18073=CARTESIAN_POINT('',(-1.26571495954046,0.4,0.524276302340173));
#18074=CARTESIAN_POINT('',(-1.26571495954046,0.4,0.524276302340173));
#18075=CARTESIAN_POINT('',(-1.26571495954046,0.4,0.524276302340173));
#18076=CARTESIAN_POINT('Origin',(-1.31100825995313,0.4,0.397690007838613));
#18077=CARTESIAN_POINT('',(-1.31100825995313,0.4,0.397690007838613));
#18078=CARTESIAN_POINT('',(-1.31100825995313,0.4,0.397690007838613));
#18079=CARTESIAN_POINT('',(-1.31100825995313,1.,0.397690007838613));
#18080=CARTESIAN_POINT('',(-1.29968493484996,1.,0.429336581464004));
#18081=CARTESIAN_POINT('',(-1.31100825995313,0.4,0.397690007838613));
#18082=CARTESIAN_POINT('Origin',(-1.34367583415243,0.4,0.267273741162095));
#18083=CARTESIAN_POINT('',(-1.34367583415243,0.4,0.267273741162095));
#18084=CARTESIAN_POINT('',(-1.34367583415243,0.4,0.267273741162095));
#18085=CARTESIAN_POINT('',(-1.34367583415243,1.,0.267273741162095));
#18086=CARTESIAN_POINT('',(-1.3355089406026,1.,0.299877807831225));
#18087=CARTESIAN_POINT('',(-1.34367583415243,0.4,0.267273741162095));
#18088=CARTESIAN_POINT('Origin',(-1.36340307554091,0.4,0.134283482251498));
#18089=CARTESIAN_POINT('',(-1.36340307554091,0.4,0.134283482251498));
#18090=CARTESIAN_POINT('',(-1.36340307554091,0.4,0.134283482251498));
#18091=CARTESIAN_POINT('',(-1.36340307554091,1.,0.134283482251498));
#18092=CARTESIAN_POINT('',(-1.35847126519379,1.,0.167531046979148));
#18093=CARTESIAN_POINT('',(-1.36340307554091,0.4,0.134283482251498));
#18094=CARTESIAN_POINT('Origin',(-1.37,0.4,-3.33066907387547E-16));
#18095=CARTESIAN_POINT('',(-1.37,0.4,-3.33066907387547E-16));
#18096=CARTESIAN_POINT('',(-1.37,0.4,-3.33066907387547E-16));
#18097=CARTESIAN_POINT('',(-1.37,1.,-3.33066907387547E-16));
#18098=CARTESIAN_POINT('',(-1.36835076888523,1.,0.0335708705628729));
#18099=CARTESIAN_POINT('',(-1.37,0.4,-3.33066907387547E-16));
#18100=CARTESIAN_POINT('Origin',(-1.36340307554091,0.4,-0.134283482251498));
#18101=CARTESIAN_POINT('',(-1.36340307554091,0.4,-0.134283482251498));
#18102=CARTESIAN_POINT('',(-1.36340307554091,0.4,-0.134283482251498));
#18103=CARTESIAN_POINT('',(-1.36340307554091,1.,-0.134283482251498));
#18104=CARTESIAN_POINT('',(-1.36505230665568,1.,-0.100712611688622));
#18105=CARTESIAN_POINT('',(-1.36340307554091,0.4,-0.134283482251498));
#18106=CARTESIAN_POINT('Origin',(-1.34367583415243,0.4,-0.267273741162096));
#18107=CARTESIAN_POINT('',(-1.34367583415243,0.4,-0.267273741162096));
#18108=CARTESIAN_POINT('',(-1.34367583415243,0.4,-0.267273741162096));
#18109=CARTESIAN_POINT('',(-1.34367583415243,1.,-0.267273741162096));
#18110=CARTESIAN_POINT('',(-1.34860764449955,1.,-0.234026176434447));
#18111=CARTESIAN_POINT('',(-1.34367583415243,0.4,-0.267273741162096));
#18112=CARTESIAN_POINT('Origin',(-1.31100825995313,0.4,-0.397690007838614));
#18113=CARTESIAN_POINT('',(-1.31100825995313,0.4,-0.397690007838614));
#18114=CARTESIAN_POINT('',(-1.31100825995313,0.4,-0.397690007838614));
#18115=CARTESIAN_POINT('',(-1.31100825995313,1.,-0.397690007838614));
#18116=CARTESIAN_POINT('',(-1.31917515350295,1.,-0.365085941169485));
#18117=CARTESIAN_POINT('',(-1.31100825995313,0.4,-0.397690007838614));
#18118=CARTESIAN_POINT('Origin',(-1.26571495954046,0.4,-0.524276302340173));
#18119=CARTESIAN_POINT('',(-1.26571495954046,0.4,-0.524276302340173));
#18120=CARTESIAN_POINT('',(-1.26571495954046,0.4,-0.524276302340173));
#18121=CARTESIAN_POINT('',(-1.27703828464363,1.,-0.492629728714784));
#18122=CARTESIAN_POINT('',(-1.26571495954046,0.4,-0.524276302340173));
#18123=CARTESIAN_POINT('Origin',(-0.739103626009029,0.4,-0.306146745892072));
#18124=CARTESIAN_POINT('',(-0.739103626009029,0.4,-0.306146745892072));
#18125=CARTESIAN_POINT('Origin',(-1.05455181300451,0.4,-3.33066907387547E-16));
#18126=CARTESIAN_POINT('Origin',(0.,1.,0.));
#18127=CARTESIAN_POINT('Origin',(0.,1.,0.));
#18128=CARTESIAN_POINT('Origin',(0.,1.,0.));
#18129=CARTESIAN_POINT('Origin',(0.,1.,0.));
#18130=CARTESIAN_POINT('Origin',(0.,1.,0.));
#18131=CARTESIAN_POINT('Origin',(0.,1.,0.));
#18132=CARTESIAN_POINT('Origin',(0.,1.,0.));
#18133=CARTESIAN_POINT('Origin',(0.,1.,0.));
#18134=CARTESIAN_POINT('Origin',(0.,1.,0.));
#18135=CARTESIAN_POINT('Origin',(0.,1.,0.));
#18136=CARTESIAN_POINT('Origin',(0.,1.,0.));
#18137=CARTESIAN_POINT('Origin',(0.,1.,0.));
#18138=CARTESIAN_POINT('Origin',(0.,1.,0.));
#18139=CARTESIAN_POINT('Origin',(0.,1.,0.));
#18140=CARTESIAN_POINT('Origin',(0.,1.,0.));
#18141=CARTESIAN_POINT('Origin',(0.,1.,0.));
#18142=CARTESIAN_POINT('Origin',(0.583891258158269,0.4,-0.546873841618297));
#18143=CARTESIAN_POINT('',(0.583891258158269,0.4,-0.546873841618297));
#18144=CARTESIAN_POINT('',(0.634682672232988,0.4,-0.487009143206976));
#18145=CARTESIAN_POINT('',(0.583891258158269,0.4,-0.546873841618297));
#18146=CARTESIAN_POINT('',(0.634682672232988,0.4,-0.487009143206976));
#18147=CARTESIAN_POINT('',(0.583891258158269,0.4,-0.546873841618297));
#18148=CARTESIAN_POINT('Origin',(0.527476652080055,0.4,-0.601471845983182));
#18149=CARTESIAN_POINT('',(0.527476652080055,0.4,-0.601471845983182));
#18150=CARTESIAN_POINT('',(0.527476652080055,0.4,-0.601471845983182));
#18151=CARTESIAN_POINT('',(0.527476652080055,0.4,-0.601471845983182));
#18152=CARTESIAN_POINT('Origin',(0.465982157494242,0.4,-0.650277347673292));
#18153=CARTESIAN_POINT('',(0.465982157494242,0.4,-0.650277347673292));
#18154=CARTESIAN_POINT('',(0.465982157494242,0.4,-0.650277347673292));
#18155=CARTESIAN_POINT('',(0.465982157494242,0.4,-0.650277347673292));
#18156=CARTESIAN_POINT('Origin',(0.4,0.4,-0.692820323027551));
#18157=CARTESIAN_POINT('',(0.4,0.4,-0.692820323027551));
#18158=CARTESIAN_POINT('',(0.4,0.4,-0.692820323027551));
#18159=CARTESIAN_POINT('',(0.4,0.4,-0.692820323027551));
#18160=CARTESIAN_POINT('Origin',(0.330165623843516,0.4,-0.728691059936941));
#18161=CARTESIAN_POINT('',(0.330165623843516,0.4,-0.728691059936941));
#18162=CARTESIAN_POINT('',(0.330165623843516,0.4,-0.728691059936941));
#18163=CARTESIAN_POINT('',(0.330165623843516,0.4,-0.728691059936941));
#18164=CARTESIAN_POINT('Origin',(0.257151572242529,0.4,-0.757544103596084));
#18165=CARTESIAN_POINT('',(0.257151572242529,0.4,-0.757544103596084));
#18166=CARTESIAN_POINT('',(0.257151572242529,0.4,-0.757544103596084));
#18167=CARTESIAN_POINT('',(0.257151572242529,0.4,-0.757544103596084));
#18168=CARTESIAN_POINT('Origin',(0.181661010427499,0.4,-0.779101583421867));
#18169=CARTESIAN_POINT('',(0.181661010427499,0.4,-0.779101583421867));
#18170=CARTESIAN_POINT('',(0.181661010427499,0.4,-0.779101583421867));
#18171=CARTESIAN_POINT('',(0.181661010427499,0.4,-0.779101583421867));
#18172=CARTESIAN_POINT('Origin',(0.104420953776041,0.4,-0.793155889099048));
#18173=CARTESIAN_POINT('',(0.104420953776041,0.4,-0.793155889099048));
#18174=CARTESIAN_POINT('',(0.104420953776041,0.4,-0.793155889099048));
#18175=CARTESIAN_POINT('',(0.104420953776041,0.4,-0.793155889099048));
#18176=CARTESIAN_POINT('Origin',(0.178820883341471,0.4,-1.35827946008212));
#18177=CARTESIAN_POINT('',(0.178820883341471,0.4,-1.35827946008212));
#18178=CARTESIAN_POINT('',(0.178820883341471,0.4,-1.35827946008212));
#18179=CARTESIAN_POINT('',(0.178820883341471,0.4,-1.35827946008212));
#18180=CARTESIAN_POINT('Origin',(0.311094480357091,0.4,-1.33421146160995));
#18181=CARTESIAN_POINT('',(0.311094480357091,0.4,-1.33421146160995));
#18182=CARTESIAN_POINT('',(0.311094480357091,0.4,-1.33421146160995));
#18183=CARTESIAN_POINT('',(0.311094480357092,1.,-1.33421146160995));
#18184=CARTESIAN_POINT('',(0.278026081103186,1.,-1.34022846122799));
#18185=CARTESIAN_POINT('',(0.311094480357091,0.4,-1.33421146160995));
#18186=CARTESIAN_POINT('Origin',(0.440372067465332,0.4,-1.29729427740829));
#18187=CARTESIAN_POINT('',(0.440372067465332,0.4,-1.29729427740829));
#18188=CARTESIAN_POINT('',(0.440372067465332,0.4,-1.29729427740829));
#18189=CARTESIAN_POINT('',(0.440372067465332,1.,-1.29729427740829));
#18190=CARTESIAN_POINT('',(0.408052670688271,1.,-1.30652357345871));
#18191=CARTESIAN_POINT('',(0.440372067465332,0.4,-1.29729427740829));
#18192=CARTESIAN_POINT('Origin',(0.565408630832021,0.4,-1.24788344014201));
#18193=CARTESIAN_POINT('',(0.565408630832021,0.4,-1.24788344014201));
#18194=CARTESIAN_POINT('',(0.565408630832021,0.4,-1.24788344014201));
#18195=CARTESIAN_POINT('',(0.565408630832021,1.,-1.24788344014201));
#18196=CARTESIAN_POINT('',(0.534149489990348,1.,-1.26023614945858));
#18197=CARTESIAN_POINT('',(0.565408630832021,0.4,-1.24788344014201));
#18198=CARTESIAN_POINT('Origin',(0.685,0.4,-1.18645480318468));
#18199=CARTESIAN_POINT('',(0.685,0.4,-1.18645480318468));
#18200=CARTESIAN_POINT('',(0.685,0.4,-1.18645480318468));
#18201=CARTESIAN_POINT('',(0.685,1.,-1.18645480318468));
#18202=CARTESIAN_POINT('',(0.655102157708007,1.,-1.20181196242401));
#18203=CARTESIAN_POINT('',(0.685,0.4,-1.18645480318468));
#18204=CARTESIAN_POINT('Origin',(0.797994444708889,0.4,-1.11359995789051));
#18205=CARTESIAN_POINT('',(0.797994444708889,0.4,-1.11359995789051));
#18206=CARTESIAN_POINT('',(0.797994444708889,0.4,-1.11359995789051));
#18207=CARTESIAN_POINT('',(0.797994444708889,1.,-1.11359995789051));
#18208=CARTESIAN_POINT('',(0.769745833531666,1.,-1.13181366921406));
#18209=CARTESIAN_POINT('',(0.797994444708889,0.4,-1.11359995789051));
#18210=CARTESIAN_POINT('Origin',(0.903303766687094,0.4,-1.0300205362462));
#18211=CARTESIAN_POINT('',(0.903303766687094,0.4,-1.0300205362462));
#18212=CARTESIAN_POINT('',(0.903303766687094,0.4,-1.0300205362462));
#18213=CARTESIAN_POINT('',(0.903303766687094,1.,-1.0300205362462));
#18214=CARTESIAN_POINT('',(0.876976436192544,1.,-1.05091539165728));
#18215=CARTESIAN_POINT('',(0.903303766687094,0.4,-1.0300205362462));
#18216=CARTESIAN_POINT('Origin',(0.999913779596035,0.4,-0.936521453771333));
#18217=CARTESIAN_POINT('',(0.999913779596035,0.4,-0.936521453771333));
#18218=CARTESIAN_POINT('',(0.999913779596035,0.4,-0.936521453771333));
#18219=CARTESIAN_POINT('',(0.999913779596035,1.,-0.936521453771333));
#18220=CARTESIAN_POINT('',(0.9757612763688,1.,-0.959896224390049));
#18221=CARTESIAN_POINT('',(0.999913779596035,0.4,-0.936521453771333));
#18222=CARTESIAN_POINT('Origin',(1.08689407619899,0.4,-0.834003157741947));
#18223=CARTESIAN_POINT('',(1.08689407619899,0.4,-0.834003157741947));
#18224=CARTESIAN_POINT('',(1.08689407619899,0.4,-0.834003157741947));
#18225=CARTESIAN_POINT('',(1.06514900204825,1.,-0.859632731749293));
#18226=CARTESIAN_POINT('',(1.08689407619899,0.4,-0.834003157741947));
#18227=CARTESIAN_POINT('Origin',(0.634682672232988,0.4,-0.487009143206976));
#18228=CARTESIAN_POINT('',(0.634682672232988,0.4,-0.487009143206976));
#18229=CARTESIAN_POINT('Origin',(0.527275906502257,0.4,-0.913268659668847));
#18230=CARTESIAN_POINT('Origin',(0.,1.,0.));
#18231=CARTESIAN_POINT('Origin',(0.,1.,0.));
#18232=CARTESIAN_POINT('Origin',(0.,1.,0.));
#18233=CARTESIAN_POINT('Origin',(0.,1.,0.));
#18234=CARTESIAN_POINT('Origin',(0.,1.,0.));
#18235=CARTESIAN_POINT('Origin',(0.,1.,0.));
#18236=CARTESIAN_POINT('Origin',(0.,1.,0.));
#18237=CARTESIAN_POINT('Origin',(0.,1.,0.));
#18238=CARTESIAN_POINT('Origin',(0.,1.,0.));
#18239=CARTESIAN_POINT('Origin',(0.,1.,0.));
#18240=CARTESIAN_POINT('Origin',(0.,1.,0.));
#18241=CARTESIAN_POINT('Origin',(0.,1.,0.));
#18242=CARTESIAN_POINT('Origin',(0.,1.,0.));
#18243=CARTESIAN_POINT('Origin',(0.,1.,0.));
#18244=CARTESIAN_POINT('Origin',(0.,1.,0.));
#18245=CARTESIAN_POINT('Origin',(0.,1.,0.));
#18246=CARTESIAN_POINT('Origin',(0.,1.,0.));
#18247=CARTESIAN_POINT('',(-0.685,2.05,1.18645480318468));
#18248=CARTESIAN_POINT('Origin',(0.,2.05,0.));
#18249=CARTESIAN_POINT('',(-0.685,1.,1.18645480318468));
#18250=CARTESIAN_POINT('Origin',(0.,2.05,0.));
#18251=CARTESIAN_POINT('',(0.,0.,0.));
#18252=CARTESIAN_POINT('Origin',(0.,-0.4,0.));
#18253=CARTESIAN_POINT('',(0.0994453842185998,-0.4,0.809917659739319));
#18254=CARTESIAN_POINT('',(0.099567253562005,-0.4,0.81091020589096));
#18255=CARTESIAN_POINT('',(0.0818108902278751,-0.4,0.666296231596819));
#18256=CARTESIAN_POINT('',(0.0663886785289718,-0.4,0.813294868644317));
#18257=CARTESIAN_POINT('',(0.091181207796194,-0.4,0.810761961965568));
#18258=CARTESIAN_POINT('',(0.0332218842499737,-0.4,0.815323436684413));
#18259=CARTESIAN_POINT('',(0.0580969799592227,-0.4,0.813802010654341));
#18260=CARTESIAN_POINT('',(-4.9960036108132E-16,-0.4,0.816));
#18261=CARTESIAN_POINT('',(0.0249164131874799,-0.4,0.81549257751331));
#18262=CARTESIAN_POINT('',(-0.0332218842499747,-0.4,0.815323436684413));
#18263=CARTESIAN_POINT('',(-0.00830547106249374,-0.4,0.815830859171103));
#18264=CARTESIAN_POINT('',(-0.0663886785289729,-0.4,0.813294868644317));
#18265=CARTESIAN_POINT('',(-0.0415135828197248,-0.4,0.814816294674389));
#18266=CARTESIAN_POINT('',(-0.0994453842186008,-0.4,0.809917659739319));
#18267=CARTESIAN_POINT('',(-0.074652854951381,-0.4,0.812450566418067));
#18268=CARTESIAN_POINT('',(-0.099567253562006,-0.4,0.81091020589096));
#18269=CARTESIAN_POINT('',(-0.0497226921093004,-0.4,0.404958829869659));
#18270=CARTESIAN_POINT('',(-0.652485211708638,-0.4,0.491682873915223));
#18271=CARTESIAN_POINT('Origin',(0.,-0.4,0.));
#18272=CARTESIAN_POINT('',(-0.651686576198591,-0.4,0.491081058892071));
#18273=CARTESIAN_POINT('',(-0.536124017894748,-0.4,0.40399842504197));
#18274=CARTESIAN_POINT('',(-0.671139677749021,-0.4,0.464141716451927));
#18275=CARTESIAN_POINT('',(-0.656549851586198,-0.4,0.484346223282036));
#18276=CARTESIAN_POINT('',(-0.689479866344548,-0.4,0.43643271406427));
#18277=CARTESIAN_POINT('',(-0.675724724897902,-0.4,0.457214465855013));
#18278=CARTESIAN_POINT('',(-0.706676729488102,-0.4,0.408));
#18279=CARTESIAN_POINT('',(-0.693779082130436,-0.4,0.429324535548202));
#18280=CARTESIAN_POINT('',(-0.722701750594522,-0.4,0.378890722620142));
#18281=CARTESIAN_POINT('',(-0.710682984764707,-0.4,0.400722680655036));
#18282=CARTESIAN_POINT('',(-0.737528356277993,-0.4,0.34915315219239));
#18283=CARTESIAN_POINT('',(-0.72640840201539,-0.4,0.371456330013204));
#18284=CARTESIAN_POINT('',(-0.751131960417191,-0.4,0.318836600847247));
#18285=CARTESIAN_POINT('',(-0.740929257312793,-0.4,0.341574014356103));
#18286=CARTESIAN_POINT('',(-0.752052465270644,-0.4,0.319227331975736));
#18287=CARTESIAN_POINT('',(-0.375565980208596,-0.4,0.159418300423624));
#18288=CARTESIAN_POINT('',(-0.752052465270644,-0.4,-0.319227331975737));
#18289=CARTESIAN_POINT('Origin',(0.,-0.4,0.));
#18290=CARTESIAN_POINT('',(-0.751131960417191,-0.4,-0.318836600847248));
#18291=CARTESIAN_POINT('',(-0.617934908122623,-0.4,-0.26229780655485));
#18292=CARTESIAN_POINT('',(-0.737528356277993,-0.4,-0.34915315219239));
#18293=CARTESIAN_POINT('',(-0.747731059382392,-0.4,-0.326415738683532));
#18294=CARTESIAN_POINT('',(-0.722701750594522,-0.4,-0.378890722620143));
#18295=CARTESIAN_POINT('',(-0.733821704857125,-0.4,-0.356587544799328));
#18296=CARTESIAN_POINT('',(-0.706676729488102,-0.4,-0.408));
#18297=CARTESIAN_POINT('',(-0.718695495317917,-0.4,-0.386168041965107));
#18298=CARTESIAN_POINT('',(-0.689479866344548,-0.4,-0.43643271406427));
#18299=CARTESIAN_POINT('',(-0.702377513702213,-0.4,-0.415108178516068));
#18300=CARTESIAN_POINT('',(-0.67113967774902,-0.4,-0.464141716451927));
#18301=CARTESIAN_POINT('',(-0.684894819195665,-0.4,-0.443359964661185));
#18302=CARTESIAN_POINT('',(-0.651686576198591,-0.4,-0.491081058892072));
#18303=CARTESIAN_POINT('',(-0.666276402361412,-0.4,-0.470876552061964));
#18304=CARTESIAN_POINT('',(-0.652485211708638,-0.4,-0.491682873915224));
#18305=CARTESIAN_POINT('',(-0.325843288099295,-0.4,-0.245540529446036));
#18306=CARTESIAN_POINT('',(-0.0995672535620054,-0.4,-0.81091020589096));
#18307=CARTESIAN_POINT('Origin',(0.,-0.4,0.));
#18308=CARTESIAN_POINT('',(-0.0994453842186002,-0.4,-0.809917659739319));
#18309=CARTESIAN_POINT('',(-0.0818108902278754,-0.4,-0.666296231596819));
#18310=CARTESIAN_POINT('',(-0.0663886785289722,-0.4,-0.813294868644317));
#18311=CARTESIAN_POINT('',(-0.0911812077961943,-0.4,-0.810761961965568));
#18312=CARTESIAN_POINT('',(-0.033221884249974,-0.4,-0.815323436684413));
#18313=CARTESIAN_POINT('',(-0.0580969799592231,-0.4,-0.813802010654341));
#18314=CARTESIAN_POINT('',(2.22044604925031E-16,-0.4,-0.816));
#18315=CARTESIAN_POINT('',(-0.0249164131874803,-0.4,-0.81549257751331));
#18316=CARTESIAN_POINT('',(0.0332218842499744,-0.4,-0.815323436684413));
#18317=CARTESIAN_POINT('',(0.00830547106249352,-0.4,-0.815830859171103));
#18318=CARTESIAN_POINT('',(0.0663886785289726,-0.4,-0.813294868644317));
#18319=CARTESIAN_POINT('',(0.0415135828197244,-0.4,-0.814816294674389));
#18320=CARTESIAN_POINT('',(0.0994453842186005,-0.4,-0.809917659739319));
#18321=CARTESIAN_POINT('',(0.0746528549513807,-0.4,-0.812450566418067));
#18322=CARTESIAN_POINT('',(0.0995672535620056,-0.4,-0.81091020589096));
#18323=CARTESIAN_POINT('',(0.0497226921093002,-0.4,-0.404958829869659));
#18324=CARTESIAN_POINT('',(0.652485211708638,-0.4,-0.491682873915223));
#18325=CARTESIAN_POINT('Origin',(0.,-0.4,0.));
#18326=CARTESIAN_POINT('',(0.651686576198591,-0.4,-0.491081058892071));
#18327=CARTESIAN_POINT('',(0.536124017894748,-0.4,-0.40399842504197));
#18328=CARTESIAN_POINT('',(0.67113967774902,-0.4,-0.464141716451927));
#18329=CARTESIAN_POINT('',(0.656549851586198,-0.4,-0.484346223282036));
#18330=CARTESIAN_POINT('',(0.689479866344548,-0.4,-0.43643271406427));
#18331=CARTESIAN_POINT('',(0.675724724897902,-0.4,-0.457214465855013));
#18332=CARTESIAN_POINT('',(0.706676729488102,-0.4,-0.408));
#18333=CARTESIAN_POINT('',(0.693779082130436,-0.4,-0.429324535548202));
#18334=CARTESIAN_POINT('',(0.722701750594522,-0.4,-0.378890722620142));
#18335=CARTESIAN_POINT('',(0.710682984764707,-0.4,-0.400722680655036));
#18336=CARTESIAN_POINT('',(0.737528356277993,-0.4,-0.34915315219239));
#18337=CARTESIAN_POINT('',(0.72640840201539,-0.4,-0.371456330013204));
#18338=CARTESIAN_POINT('',(0.751131960417191,-0.4,-0.318836600847247));
#18339=CARTESIAN_POINT('',(0.740929257312793,-0.4,-0.341574014356103));
#18340=CARTESIAN_POINT('',(0.752052465270644,-0.4,-0.319227331975737));
#18341=CARTESIAN_POINT('',(0.375565980208596,-0.4,-0.159418300423624));
#18342=CARTESIAN_POINT('',(0.752052465270643,-0.4,0.319227331975737));
#18343=CARTESIAN_POINT('Origin',(0.,-0.4,0.));
#18344=CARTESIAN_POINT('',(0.751131960417191,-0.4,0.318836600847248));
#18345=CARTESIAN_POINT('',(0.617934908122623,-0.4,0.26229780655485));
#18346=CARTESIAN_POINT('',(0.737528356277993,-0.4,0.349153152192391));
#18347=CARTESIAN_POINT('',(0.747731059382392,-0.4,0.326415738683533));
#18348=CARTESIAN_POINT('',(0.722701750594521,-0.4,0.378890722620143));
#18349=CARTESIAN_POINT('',(0.733821704857125,-0.4,0.356587544799328));
#18350=CARTESIAN_POINT('',(0.706676729488102,-0.4,0.408000000000001));
#18351=CARTESIAN_POINT('',(0.718695495317916,-0.4,0.386168041965108));
#18352=CARTESIAN_POINT('',(0.689479866344547,-0.4,0.436432714064271));
#18353=CARTESIAN_POINT('',(0.702377513702213,-0.4,0.415108178516068));
#18354=CARTESIAN_POINT('',(0.67113967774902,-0.4,0.464141716451928));
#18355=CARTESIAN_POINT('',(0.684894819195665,-0.4,0.443359964661185));
#18356=CARTESIAN_POINT('',(0.65168657619859,-0.4,0.491081058892072));
#18357=CARTESIAN_POINT('',(0.666276402361412,-0.4,0.470876552061965));
#18358=CARTESIAN_POINT('',(0.652485211708638,-0.4,0.491682873915224));
#18359=CARTESIAN_POINT('',(0.325843288099295,-0.4,0.245540529446036));
#18360=CARTESIAN_POINT('Origin',(0.,-0.4,0.));
#18361=CARTESIAN_POINT('Origin',(0.,0.,0.));
#18362=CARTESIAN_POINT('',(0.752052465270644,0.4,-0.319227331975737));
#18363=CARTESIAN_POINT('',(0.752052465270644,0.,-0.319227331975737));
#18364=CARTESIAN_POINT('',(0.752052465270643,0.4,0.319227331975737));
#18365=CARTESIAN_POINT('Origin',(0.,0.4,0.));
#18366=CARTESIAN_POINT('',(0.752052465270643,0.,0.319227331975737));
#18367=CARTESIAN_POINT('Origin',(0.,0.,0.));
#18368=CARTESIAN_POINT('',(-0.099567253562006,0.4,0.81091020589096));
#18369=CARTESIAN_POINT('',(-0.099567253562006,0.,0.81091020589096));
#18370=CARTESIAN_POINT('',(-0.652485211708638,0.4,0.491682873915223));
#18371=CARTESIAN_POINT('Origin',(0.,0.4,0.));
#18372=CARTESIAN_POINT('',(-0.652485211708638,0.,0.491682873915223));
#18373=CARTESIAN_POINT('Origin',(0.,0.,0.));
#18374=CARTESIAN_POINT('',(-0.652485211708638,0.4,-0.491682873915224));
#18375=CARTESIAN_POINT('',(-0.652485211708638,0.,-0.491682873915224));
#18376=CARTESIAN_POINT('',(-0.0995672535620054,0.4,-0.81091020589096));
#18377=CARTESIAN_POINT('Origin',(0.,0.4,0.));
#18378=CARTESIAN_POINT('',(-0.0995672535620054,0.,-0.81091020589096));
#18379=CARTESIAN_POINT('Origin',(0.,0.,0.));
#18380=CARTESIAN_POINT('',(0.652485211708638,0.4,-0.491682873915223));
#18381=CARTESIAN_POINT('',(0.652485211708638,0.,-0.491682873915223));
#18382=CARTESIAN_POINT('',(0.0995672535620056,0.4,-0.81091020589096));
#18383=CARTESIAN_POINT('',(0.0995672535620056,0.,-0.81091020589096));
#18384=CARTESIAN_POINT('Origin',(0.,0.4,0.));
#18385=CARTESIAN_POINT('Origin',(0.,0.,0.));
#18386=CARTESIAN_POINT('',(-0.752052465270644,0.4,-0.319227331975737));
#18387=CARTESIAN_POINT('',(-0.752052465270644,0.,-0.319227331975737));
#18388=CARTESIAN_POINT('',(-0.752052465270644,0.4,0.319227331975736));
#18389=CARTESIAN_POINT('',(-0.752052465270644,0.,0.319227331975736));
#18390=CARTESIAN_POINT('Origin',(0.,0.4,0.));
#18391=CARTESIAN_POINT('Origin',(0.,0.,0.));
#18392=CARTESIAN_POINT('',(0.099567253562005,0.4,0.81091020589096));
#18393=CARTESIAN_POINT('',(0.099567253562005,0.,0.81091020589096));
#18394=CARTESIAN_POINT('',(0.652485211708638,0.4,0.491682873915224));
#18395=CARTESIAN_POINT('',(0.652485211708638,0.,0.491682873915224));
#18396=CARTESIAN_POINT('Origin',(0.,0.4,0.));
#18397=CARTESIAN_POINT('Origin',(0.,0.4,0.));
#18398=CARTESIAN_POINT('',(0.0994453842185998,0.4,0.809917659739319));
#18399=CARTESIAN_POINT('',(0.0818108902278751,0.4,0.666296231596819));
#18400=CARTESIAN_POINT('',(0.65168657619859,0.4,0.491081058892072));
#18401=CARTESIAN_POINT('',(0.325843288099295,0.4,0.245540529446036));
#18402=CARTESIAN_POINT('',(0.67113967774902,0.4,0.464141716451928));
#18403=CARTESIAN_POINT('',(0.666276402361412,0.4,0.470876552061965));
#18404=CARTESIAN_POINT('',(0.689479866344547,0.4,0.436432714064271));
#18405=CARTESIAN_POINT('',(0.684894819195665,0.4,0.443359964661185));
#18406=CARTESIAN_POINT('',(0.706676729488102,0.4,0.408000000000001));
#18407=CARTESIAN_POINT('',(0.702377513702213,0.4,0.415108178516068));
#18408=CARTESIAN_POINT('',(0.722701750594521,0.4,0.378890722620143));
#18409=CARTESIAN_POINT('',(0.718695495317916,0.4,0.386168041965108));
#18410=CARTESIAN_POINT('',(0.737528356277993,0.4,0.349153152192391));
#18411=CARTESIAN_POINT('',(0.733821704857125,0.4,0.356587544799328));
#18412=CARTESIAN_POINT('',(0.751131960417191,0.4,0.318836600847248));
#18413=CARTESIAN_POINT('',(0.747731059382392,0.4,0.326415738683533));
#18414=CARTESIAN_POINT('',(0.617934908122623,0.4,0.26229780655485));
#18415=CARTESIAN_POINT('',(0.751131960417191,0.4,-0.318836600847247));
#18416=CARTESIAN_POINT('',(0.375565980208596,0.4,-0.159418300423624));
#18417=CARTESIAN_POINT('',(0.737528356277993,0.4,-0.34915315219239));
#18418=CARTESIAN_POINT('',(0.740929257312793,0.4,-0.341574014356103));
#18419=CARTESIAN_POINT('',(0.722701750594522,0.4,-0.378890722620142));
#18420=CARTESIAN_POINT('',(0.72640840201539,0.4,-0.371456330013204));
#18421=CARTESIAN_POINT('',(0.706676729488102,0.4,-0.408));
#18422=CARTESIAN_POINT('',(0.710682984764707,0.4,-0.400722680655036));
#18423=CARTESIAN_POINT('',(0.689479866344548,0.4,-0.43643271406427));
#18424=CARTESIAN_POINT('',(0.693779082130436,0.4,-0.429324535548202));
#18425=CARTESIAN_POINT('',(0.67113967774902,0.4,-0.464141716451927));
#18426=CARTESIAN_POINT('',(0.675724724897902,0.4,-0.457214465855013));
#18427=CARTESIAN_POINT('',(0.651686576198591,0.4,-0.491081058892071));
#18428=CARTESIAN_POINT('',(0.656549851586198,0.4,-0.484346223282036));
#18429=CARTESIAN_POINT('',(0.536124017894748,0.4,-0.40399842504197));
#18430=CARTESIAN_POINT('',(0.0994453842186005,0.4,-0.809917659739319));
#18431=CARTESIAN_POINT('',(0.0497226921093002,0.4,-0.404958829869659));
#18432=CARTESIAN_POINT('',(0.0663886785289726,0.4,-0.813294868644317));
#18433=CARTESIAN_POINT('',(0.0746528549513807,0.4,-0.812450566418067));
#18434=CARTESIAN_POINT('',(0.0332218842499744,0.4,-0.815323436684413));
#18435=CARTESIAN_POINT('',(0.0415135828197244,0.4,-0.814816294674389));
#18436=CARTESIAN_POINT('',(2.22044604925031E-16,0.4,-0.816));
#18437=CARTESIAN_POINT('',(0.00830547106249352,0.4,-0.815830859171103));
#18438=CARTESIAN_POINT('',(-0.033221884249974,0.4,-0.815323436684413));
#18439=CARTESIAN_POINT('',(-0.0249164131874803,0.4,-0.81549257751331));
#18440=CARTESIAN_POINT('',(-0.0663886785289722,0.4,-0.813294868644317));
#18441=CARTESIAN_POINT('',(-0.0580969799592231,0.4,-0.813802010654341));
#18442=CARTESIAN_POINT('',(-0.0994453842186002,0.4,-0.809917659739319));
#18443=CARTESIAN_POINT('',(-0.0911812077961943,0.4,-0.810761961965568));
#18444=CARTESIAN_POINT('',(-0.0818108902278754,0.4,-0.666296231596819));
#18445=CARTESIAN_POINT('',(-0.651686576198591,0.4,-0.491081058892072));
#18446=CARTESIAN_POINT('',(-0.325843288099295,0.4,-0.245540529446036));
#18447=CARTESIAN_POINT('',(-0.67113967774902,0.4,-0.464141716451927));
#18448=CARTESIAN_POINT('',(-0.666276402361412,0.4,-0.470876552061964));
#18449=CARTESIAN_POINT('',(-0.689479866344548,0.4,-0.43643271406427));
#18450=CARTESIAN_POINT('',(-0.684894819195665,0.4,-0.443359964661185));
#18451=CARTESIAN_POINT('',(-0.706676729488102,0.4,-0.408));
#18452=CARTESIAN_POINT('',(-0.702377513702213,0.4,-0.415108178516068));
#18453=CARTESIAN_POINT('',(-0.722701750594522,0.4,-0.378890722620143));
#18454=CARTESIAN_POINT('',(-0.718695495317917,0.4,-0.386168041965107));
#18455=CARTESIAN_POINT('',(-0.737528356277993,0.4,-0.34915315219239));
#18456=CARTESIAN_POINT('',(-0.733821704857125,0.4,-0.356587544799328));
#18457=CARTESIAN_POINT('',(-0.751131960417191,0.4,-0.318836600847248));
#18458=CARTESIAN_POINT('',(-0.747731059382392,0.4,-0.326415738683532));
#18459=CARTESIAN_POINT('',(-0.617934908122623,0.4,-0.26229780655485));
#18460=CARTESIAN_POINT('',(-0.751131960417191,0.4,0.318836600847247));
#18461=CARTESIAN_POINT('',(-0.375565980208596,0.4,0.159418300423624));
#18462=CARTESIAN_POINT('',(-0.737528356277993,0.4,0.34915315219239));
#18463=CARTESIAN_POINT('',(-0.740929257312793,0.4,0.341574014356103));
#18464=CARTESIAN_POINT('',(-0.722701750594522,0.4,0.378890722620142));
#18465=CARTESIAN_POINT('',(-0.72640840201539,0.4,0.371456330013204));
#18466=CARTESIAN_POINT('',(-0.706676729488102,0.4,0.408));
#18467=CARTESIAN_POINT('',(-0.710682984764707,0.4,0.400722680655036));
#18468=CARTESIAN_POINT('',(-0.689479866344548,0.4,0.43643271406427));
#18469=CARTESIAN_POINT('',(-0.693779082130436,0.4,0.429324535548202));
#18470=CARTESIAN_POINT('',(-0.671139677749021,0.4,0.464141716451927));
#18471=CARTESIAN_POINT('',(-0.675724724897902,0.4,0.457214465855013));
#18472=CARTESIAN_POINT('',(-0.651686576198591,0.4,0.491081058892071));
#18473=CARTESIAN_POINT('',(-0.656549851586198,0.4,0.484346223282036));
#18474=CARTESIAN_POINT('',(-0.536124017894748,0.4,0.40399842504197));
#18475=CARTESIAN_POINT('',(-0.0994453842186008,0.4,0.809917659739319));
#18476=CARTESIAN_POINT('',(-0.0497226921093004,0.4,0.404958829869659));
#18477=CARTESIAN_POINT('',(-0.0663886785289729,0.4,0.813294868644317));
#18478=CARTESIAN_POINT('',(-0.074652854951381,0.4,0.812450566418067));
#18479=CARTESIAN_POINT('',(-0.0332218842499747,0.4,0.815323436684413));
#18480=CARTESIAN_POINT('',(-0.0415135828197248,0.4,0.814816294674389));
#18481=CARTESIAN_POINT('',(-4.9960036108132E-16,0.4,0.816));
#18482=CARTESIAN_POINT('',(-0.00830547106249374,0.4,0.815830859171103));
#18483=CARTESIAN_POINT('',(0.0332218842499737,0.4,0.815323436684413));
#18484=CARTESIAN_POINT('',(0.0249164131874799,0.4,0.81549257751331));
#18485=CARTESIAN_POINT('',(0.0663886785289718,0.4,0.813294868644317));
#18486=CARTESIAN_POINT('',(0.0580969799592227,0.4,0.813802010654341));
#18487=CARTESIAN_POINT('',(0.091181207796194,0.4,0.810761961965568));
#18488=CARTESIAN_POINT('Origin',(1.23586981624525,0.,0.5245956131097));
#18489=CARTESIAN_POINT('',(0.751131960417191,1.,0.318836600847248));
#18490=CARTESIAN_POINT('',(0.751131960417191,0.,0.318836600847248));
#18491=CARTESIAN_POINT('',(1.23586981624525,1.,0.5245956131097));
#18492=CARTESIAN_POINT('',(1.23586981624525,1.,0.5245956131097));
#18493=CARTESIAN_POINT('',(1.23586981624525,-1.,0.5245956131097));
#18494=CARTESIAN_POINT('',(1.23586981624525,0.,0.5245956131097));
#18495=CARTESIAN_POINT('',(0.751131960417191,-1.,0.318836600847248));
#18496=CARTESIAN_POINT('',(1.23586981624525,-1.,0.5245956131097));
#18497=CARTESIAN_POINT('',(0.751131960417191,0.,0.318836600847248));
#18498=CARTESIAN_POINT('Origin',(0.751131960417191,0.,0.318836600847248));
#18499=CARTESIAN_POINT('',(0.737528356277993,1.,0.349153152192391));
#18500=CARTESIAN_POINT('',(0.737528356277993,0.,0.349153152192391));
#18501=CARTESIAN_POINT('',(0.751131960417191,1.,0.318836600847248));
#18502=CARTESIAN_POINT('Origin',(0.751131960417191,0.,0.318836600847248));
#18503=CARTESIAN_POINT('',(0.737528356277993,-1.,0.349153152192391));
#18504=CARTESIAN_POINT('',(0.751131960417191,-1.,0.318836600847248));
#18505=CARTESIAN_POINT('',(0.737528356277993,0.,0.349153152192391));
#18506=CARTESIAN_POINT('Origin',(0.737528356277993,0.,0.349153152192391));
#18507=CARTESIAN_POINT('',(0.722701750594521,1.,0.378890722620143));
#18508=CARTESIAN_POINT('',(0.722701750594521,0.,0.378890722620143));
#18509=CARTESIAN_POINT('',(0.737528356277993,1.,0.349153152192391));
#18510=CARTESIAN_POINT('Origin',(0.722701750594521,0.,0.378890722620143));
#18511=CARTESIAN_POINT('',(0.706676729488102,1.,0.408000000000001));
#18512=CARTESIAN_POINT('',(0.706676729488102,0.,0.408000000000001));
#18513=CARTESIAN_POINT('',(0.722701750594521,1.,0.378890722620143));
#18514=CARTESIAN_POINT('Origin',(0.706676729488102,0.,0.408000000000001));
#18515=CARTESIAN_POINT('',(0.689479866344547,1.,0.436432714064271));
#18516=CARTESIAN_POINT('',(0.689479866344547,0.,0.436432714064271));
#18517=CARTESIAN_POINT('',(0.706676729488102,1.,0.408000000000001));
#18518=CARTESIAN_POINT('Origin',(0.689479866344547,0.,0.436432714064271));
#18519=CARTESIAN_POINT('',(0.67113967774902,1.,0.464141716451928));
#18520=CARTESIAN_POINT('',(0.67113967774902,0.,0.464141716451928));
#18521=CARTESIAN_POINT('',(0.689479866344547,1.,0.436432714064271));
#18522=CARTESIAN_POINT('Origin',(0.67113967774902,0.,0.464141716451928));
#18523=CARTESIAN_POINT('',(0.65168657619859,1.,0.491081058892072));
#18524=CARTESIAN_POINT('',(0.65168657619859,0.,0.491081058892072));
#18525=CARTESIAN_POINT('',(0.67113967774902,1.,0.464141716451928));
#18526=CARTESIAN_POINT('Origin',(0.932067487714439,-1.,0.53812941493483));
#18527=CARTESIAN_POINT('',(1.07224803578949,-1.,0.807996850083941));
#18528=CARTESIAN_POINT('',(0.65168657619859,-1.,0.491081058892072));
#18529=CARTESIAN_POINT('',(0.65168657619859,-1.,0.491081058892072));
#18530=CARTESIAN_POINT('',(0.67113967774902,-1.,0.464141716451928));
#18531=CARTESIAN_POINT('',(0.67113967774902,-1.,0.464141716451928));
#18532=CARTESIAN_POINT('',(0.689479866344547,-1.,0.436432714064271));
#18533=CARTESIAN_POINT('',(0.689479866344547,-1.,0.436432714064271));
#18534=CARTESIAN_POINT('',(0.706676729488102,-1.,0.408000000000001));
#18535=CARTESIAN_POINT('',(0.706676729488102,-1.,0.408000000000001));
#18536=CARTESIAN_POINT('',(0.722701750594521,-1.,0.378890722620143));
#18537=CARTESIAN_POINT('',(0.722701750594521,-1.,0.378890722620143));
#18538=CARTESIAN_POINT('',(0.737528356277993,-1.,0.349153152192391));
#18539=CARTESIAN_POINT('',(1.21348721953288,-1.,0.574476742810666));
#18540=CARTESIAN_POINT('',(1.21348721953288,-1.,0.574476742810666));
#18541=CARTESIAN_POINT('',(1.1890923656228,-1.,0.623405250232603));
#18542=CARTESIAN_POINT('',(1.1890923656228,-1.,0.623405250232603));
#18543=CARTESIAN_POINT('',(1.16272570712099,-1.,0.671300000000001));
#18544=CARTESIAN_POINT('',(1.16272570712099,-1.,0.671300000000001));
#18545=CARTESIAN_POINT('',(1.13443096636543,-1.,0.718081570959179));
#18546=CARTESIAN_POINT('',(1.13443096636543,-1.,0.718081570959179));
#18547=CARTESIAN_POINT('',(1.10425506292382,-1.,0.76367238787789));
#18548=CARTESIAN_POINT('',(1.10425506292382,-1.,0.76367238787789));
#18549=CARTESIAN_POINT('',(1.07224803578949,-1.,0.807996850083941));
#18550=CARTESIAN_POINT('Origin',(0.67113967774902,0.,0.464141716451928));
#18551=CARTESIAN_POINT('',(0.67113967774902,0.,0.464141716451928));
#18552=CARTESIAN_POINT('',(0.65168657619859,0.,0.491081058892072));
#18553=CARTESIAN_POINT('Origin',(0.689479866344547,0.,0.436432714064271));
#18554=CARTESIAN_POINT('',(0.689479866344547,0.,0.436432714064271));
#18555=CARTESIAN_POINT('Origin',(0.706676729488102,0.,0.408000000000001));
#18556=CARTESIAN_POINT('',(0.706676729488102,0.,0.408000000000001));
#18557=CARTESIAN_POINT('Origin',(0.722701750594521,0.,0.378890722620143));
#18558=CARTESIAN_POINT('',(0.722701750594521,0.,0.378890722620143));
#18559=CARTESIAN_POINT('Origin',(0.737528356277993,0.,0.349153152192391));
#18560=CARTESIAN_POINT('Origin',(1.21348721953288,0.,0.574476742810666));
#18561=CARTESIAN_POINT('',(1.21348721953288,1.,0.574476742810666));
#18562=CARTESIAN_POINT('',(1.21348721953288,1.,0.574476742810666));
#18563=CARTESIAN_POINT('',(1.21348721953288,0.,0.574476742810666));
#18564=CARTESIAN_POINT('Origin',(1.1890923656228,0.,0.623405250232603));
#18565=CARTESIAN_POINT('',(1.1890923656228,1.,0.623405250232603));
#18566=CARTESIAN_POINT('',(1.1890923656228,1.,0.623405250232603));
#18567=CARTESIAN_POINT('',(1.1890923656228,0.,0.623405250232603));
#18568=CARTESIAN_POINT('Origin',(1.16272570712099,0.,0.671300000000001));
#18569=CARTESIAN_POINT('',(1.16272570712099,1.,0.671300000000001));
#18570=CARTESIAN_POINT('',(1.16272570712099,1.,0.671300000000001));
#18571=CARTESIAN_POINT('',(1.16272570712099,0.,0.671300000000001));
#18572=CARTESIAN_POINT('Origin',(1.13443096636543,0.,0.718081570959179));
#18573=CARTESIAN_POINT('',(1.13443096636543,1.,0.718081570959179));
#18574=CARTESIAN_POINT('',(1.13443096636543,1.,0.718081570959179));
#18575=CARTESIAN_POINT('',(1.13443096636543,0.,0.718081570959179));
#18576=CARTESIAN_POINT('Origin',(1.10425506292382,0.,0.76367238787789));
#18577=CARTESIAN_POINT('',(1.10425506292382,1.,0.76367238787789));
#18578=CARTESIAN_POINT('',(1.10425506292382,1.,0.76367238787789));
#18579=CARTESIAN_POINT('',(1.10425506292382,0.,0.76367238787789));
#18580=CARTESIAN_POINT('Origin',(1.07224803578949,0.,0.807996850083941));
#18581=CARTESIAN_POINT('',(1.07224803578949,1.,0.807996850083941));
#18582=CARTESIAN_POINT('',(1.07224803578949,1.,0.807996850083941));
#18583=CARTESIAN_POINT('',(1.07224803578949,0.,0.807996850083941));
#18584=CARTESIAN_POINT('Origin',(0.65168657619859,0.,0.491081058892072));
#18585=CARTESIAN_POINT('',(0.65168657619859,1.,0.491081058892072));
#18586=CARTESIAN_POINT('Origin',(0.932067487714439,1.,0.53812941493483));
#18587=CARTESIAN_POINT('Origin',(-1.0722480357895,0.,0.80799685008394));
#18588=CARTESIAN_POINT('',(-0.651686576198591,1.,0.491081058892071));
#18589=CARTESIAN_POINT('',(-0.651686576198591,0.,0.491081058892071));
#18590=CARTESIAN_POINT('',(-1.0722480357895,1.,0.80799685008394));
#18591=CARTESIAN_POINT('',(-1.0722480357895,1.,0.80799685008394));
#18592=CARTESIAN_POINT('',(-1.0722480357895,-1.,0.80799685008394));
#18593=CARTESIAN_POINT('',(-1.0722480357895,0.,0.80799685008394));
#18594=CARTESIAN_POINT('',(-0.651686576198591,-1.,0.491081058892071));
#18595=CARTESIAN_POINT('',(-1.0722480357895,-1.,0.80799685008394));
#18596=CARTESIAN_POINT('',(-0.651686576198591,0.,0.491081058892071));
#18597=CARTESIAN_POINT('Origin',(-0.651686576198591,0.,0.491081058892071));
#18598=CARTESIAN_POINT('',(-0.671139677749021,1.,0.464141716451927));
#18599=CARTESIAN_POINT('',(-0.671139677749021,0.,0.464141716451927));
#18600=CARTESIAN_POINT('',(-0.651686576198591,1.,0.491081058892071));
#18601=CARTESIAN_POINT('Origin',(-0.651686576198591,0.,0.491081058892071));
#18602=CARTESIAN_POINT('',(-0.671139677749021,-1.,0.464141716451927));
#18603=CARTESIAN_POINT('',(-0.651686576198591,-1.,0.491081058892071));
#18604=CARTESIAN_POINT('',(-0.671139677749021,0.,0.464141716451927));
#18605=CARTESIAN_POINT('Origin',(-0.671139677749021,0.,0.464141716451927));
#18606=CARTESIAN_POINT('',(-0.689479866344548,1.,0.43643271406427));
#18607=CARTESIAN_POINT('',(-0.689479866344548,0.,0.43643271406427));
#18608=CARTESIAN_POINT('',(-0.671139677749021,1.,0.464141716451927));
#18609=CARTESIAN_POINT('Origin',(-0.689479866344548,0.,0.43643271406427));
#18610=CARTESIAN_POINT('',(-0.706676729488102,1.,0.408));
#18611=CARTESIAN_POINT('',(-0.706676729488102,0.,0.408));
#18612=CARTESIAN_POINT('',(-0.689479866344548,1.,0.43643271406427));
#18613=CARTESIAN_POINT('Origin',(-0.706676729488102,0.,0.408));
#18614=CARTESIAN_POINT('',(-0.722701750594522,1.,0.378890722620142));
#18615=CARTESIAN_POINT('',(-0.722701750594522,0.,0.378890722620142));
#18616=CARTESIAN_POINT('',(-0.706676729488102,1.,0.408));
#18617=CARTESIAN_POINT('Origin',(-0.722701750594522,0.,0.378890722620142));
#18618=CARTESIAN_POINT('',(-0.737528356277993,1.,0.34915315219239));
#18619=CARTESIAN_POINT('',(-0.737528356277993,0.,0.34915315219239));
#18620=CARTESIAN_POINT('',(-0.722701750594522,1.,0.378890722620142));
#18621=CARTESIAN_POINT('Origin',(-0.737528356277993,0.,0.34915315219239));
#18622=CARTESIAN_POINT('',(-0.751131960417191,1.,0.318836600847247));
#18623=CARTESIAN_POINT('',(-0.751131960417191,0.,0.318836600847247));
#18624=CARTESIAN_POINT('',(-0.737528356277993,1.,0.34915315219239));
#18625=CARTESIAN_POINT('Origin',(-0.932067487714439,-1.,0.538129414934829));
#18626=CARTESIAN_POINT('',(-1.23586981624525,-1.,0.524595613109699));
#18627=CARTESIAN_POINT('',(-0.751131960417191,-1.,0.318836600847247));
#18628=CARTESIAN_POINT('',(-0.751131960417191,-1.,0.318836600847247));
#18629=CARTESIAN_POINT('',(-0.737528356277993,-1.,0.34915315219239));
#18630=CARTESIAN_POINT('',(-0.737528356277993,-1.,0.34915315219239));
#18631=CARTESIAN_POINT('',(-0.722701750594522,-1.,0.378890722620142));
#18632=CARTESIAN_POINT('',(-0.722701750594522,-1.,0.378890722620142));
#18633=CARTESIAN_POINT('',(-0.706676729488102,-1.,0.408));
#18634=CARTESIAN_POINT('',(-0.706676729488102,-1.,0.408));
#18635=CARTESIAN_POINT('',(-0.689479866344548,-1.,0.43643271406427));
#18636=CARTESIAN_POINT('',(-0.689479866344548,-1.,0.43643271406427));
#18637=CARTESIAN_POINT('',(-0.671139677749021,-1.,0.464141716451927));
#18638=CARTESIAN_POINT('',(-1.10425506292382,-1.,0.763672387877888));
#18639=CARTESIAN_POINT('',(-1.10425506292382,-1.,0.763672387877888));
#18640=CARTESIAN_POINT('',(-1.13443096636543,-1.,0.718081570959177));
#18641=CARTESIAN_POINT('',(-1.13443096636543,-1.,0.718081570959177));
#18642=CARTESIAN_POINT('',(-1.16272570712099,-1.,0.6713));
#18643=CARTESIAN_POINT('',(-1.16272570712099,-1.,0.6713));
#18644=CARTESIAN_POINT('',(-1.1890923656228,-1.,0.623405250232602));
#18645=CARTESIAN_POINT('',(-1.1890923656228,-1.,0.623405250232602));
#18646=CARTESIAN_POINT('',(-1.21348721953288,-1.,0.574476742810665));
#18647=CARTESIAN_POINT('',(-1.21348721953288,-1.,0.574476742810665));
#18648=CARTESIAN_POINT('',(-1.23586981624525,-1.,0.524595613109699));
#18649=CARTESIAN_POINT('Origin',(-0.737528356277993,0.,0.34915315219239));
#18650=CARTESIAN_POINT('',(-0.737528356277993,0.,0.34915315219239));
#18651=CARTESIAN_POINT('',(-0.751131960417191,0.,0.318836600847247));
#18652=CARTESIAN_POINT('Origin',(-0.722701750594522,0.,0.378890722620142));
#18653=CARTESIAN_POINT('',(-0.722701750594522,0.,0.378890722620142));
#18654=CARTESIAN_POINT('Origin',(-0.706676729488102,0.,0.408));
#18655=CARTESIAN_POINT('',(-0.706676729488102,0.,0.408));
#18656=CARTESIAN_POINT('Origin',(-0.689479866344548,0.,0.43643271406427));
#18657=CARTESIAN_POINT('',(-0.689479866344548,0.,0.43643271406427));
#18658=CARTESIAN_POINT('Origin',(-0.671139677749021,0.,0.464141716451927));
#18659=CARTESIAN_POINT('Origin',(-1.10425506292382,0.,0.763672387877888));
#18660=CARTESIAN_POINT('',(-1.10425506292382,1.,0.763672387877888));
#18661=CARTESIAN_POINT('',(-1.10425506292382,1.,0.763672387877888));
#18662=CARTESIAN_POINT('',(-1.10425506292382,0.,0.763672387877888));
#18663=CARTESIAN_POINT('Origin',(-1.13443096636543,0.,0.718081570959177));
#18664=CARTESIAN_POINT('',(-1.13443096636543,1.,0.718081570959177));
#18665=CARTESIAN_POINT('',(-1.13443096636543,1.,0.718081570959177));
#18666=CARTESIAN_POINT('',(-1.13443096636543,0.,0.718081570959177));
#18667=CARTESIAN_POINT('Origin',(-1.16272570712099,0.,0.6713));
#18668=CARTESIAN_POINT('',(-1.16272570712099,1.,0.6713));
#18669=CARTESIAN_POINT('',(-1.16272570712099,1.,0.6713));
#18670=CARTESIAN_POINT('',(-1.16272570712099,0.,0.6713));
#18671=CARTESIAN_POINT('Origin',(-1.1890923656228,0.,0.623405250232602));
#18672=CARTESIAN_POINT('',(-1.1890923656228,1.,0.623405250232602));
#18673=CARTESIAN_POINT('',(-1.1890923656228,1.,0.623405250232602));
#18674=CARTESIAN_POINT('',(-1.1890923656228,0.,0.623405250232602));
#18675=CARTESIAN_POINT('Origin',(-1.21348721953288,0.,0.574476742810665));
#18676=CARTESIAN_POINT('',(-1.21348721953288,1.,0.574476742810665));
#18677=CARTESIAN_POINT('',(-1.21348721953288,1.,0.574476742810665));
#18678=CARTESIAN_POINT('',(-1.21348721953288,0.,0.574476742810665));
#18679=CARTESIAN_POINT('Origin',(-1.23586981624525,0.,0.524595613109699));
#18680=CARTESIAN_POINT('',(-1.23586981624525,1.,0.524595613109699));
#18681=CARTESIAN_POINT('',(-1.23586981624525,1.,0.524595613109699));
#18682=CARTESIAN_POINT('',(-1.23586981624525,0.,0.524595613109699));
#18683=CARTESIAN_POINT('Origin',(-0.751131960417191,0.,0.318836600847247));
#18684=CARTESIAN_POINT('',(-0.751131960417191,1.,0.318836600847247));
#18685=CARTESIAN_POINT('Origin',(-0.932067487714439,1.,0.538129414934829));
#18686=CARTESIAN_POINT('Origin',(-0.163621780455751,0.,-1.33259246319364));
#18687=CARTESIAN_POINT('',(-0.0994453842186002,1.,-0.809917659739319));
#18688=CARTESIAN_POINT('',(-0.0994453842186002,0.,-0.809917659739319));
#18689=CARTESIAN_POINT('',(-0.163621780455751,1.,-1.33259246319364));
#18690=CARTESIAN_POINT('',(-0.163621780455751,1.,-1.33259246319364));
#18691=CARTESIAN_POINT('',(-0.163621780455751,-1.,-1.33259246319364));
#18692=CARTESIAN_POINT('',(-0.163621780455751,0.,-1.33259246319364));
#18693=CARTESIAN_POINT('',(-0.0994453842186002,-1.,-0.809917659739319));
#18694=CARTESIAN_POINT('',(-0.163621780455751,-1.,-1.33259246319364));
#18695=CARTESIAN_POINT('',(-0.0994453842186002,0.,-0.809917659739319));
#18696=CARTESIAN_POINT('Origin',(-0.0994453842186002,0.,-0.809917659739319));
#18697=CARTESIAN_POINT('',(-0.0663886785289722,1.,-0.813294868644317));
#18698=CARTESIAN_POINT('',(-0.0663886785289722,0.,-0.813294868644317));
#18699=CARTESIAN_POINT('',(-0.0994453842186002,1.,-0.809917659739319));
#18700=CARTESIAN_POINT('Origin',(-0.0994453842186002,0.,-0.809917659739319));
#18701=CARTESIAN_POINT('',(-0.0663886785289722,-1.,-0.813294868644317));
#18702=CARTESIAN_POINT('',(-0.0994453842186002,-1.,-0.809917659739319));
#18703=CARTESIAN_POINT('',(-0.0663886785289722,0.,-0.813294868644317));
#18704=CARTESIAN_POINT('Origin',(-0.0663886785289722,0.,-0.813294868644317));
#18705=CARTESIAN_POINT('',(-0.033221884249974,1.,-0.815323436684413));
#18706=CARTESIAN_POINT('',(-0.033221884249974,0.,-0.815323436684413));
#18707=CARTESIAN_POINT('',(-0.0663886785289722,1.,-0.813294868644317));
#18708=CARTESIAN_POINT('Origin',(-0.033221884249974,0.,-0.815323436684413));
#18709=CARTESIAN_POINT('',(2.22044604925031E-16,1.,-0.816));
#18710=CARTESIAN_POINT('',(2.22044604925031E-16,0.,-0.816));
#18711=CARTESIAN_POINT('',(-0.033221884249974,1.,-0.815323436684413));
#18712=CARTESIAN_POINT('Origin',(2.22044604925031E-16,0.,-0.816));
#18713=CARTESIAN_POINT('',(0.0332218842499744,1.,-0.815323436684413));
#18714=CARTESIAN_POINT('',(0.0332218842499744,0.,-0.815323436684413));
#18715=CARTESIAN_POINT('',(2.22044604925031E-16,1.,-0.816));
#18716=CARTESIAN_POINT('Origin',(0.0332218842499744,0.,-0.815323436684413));
#18717=CARTESIAN_POINT('',(0.0663886785289726,1.,-0.813294868644317));
#18718=CARTESIAN_POINT('',(0.0663886785289726,0.,-0.813294868644317));
#18719=CARTESIAN_POINT('',(0.0332218842499744,1.,-0.815323436684413));
#18720=CARTESIAN_POINT('Origin',(0.0663886785289726,0.,-0.813294868644317));
#18721=CARTESIAN_POINT('',(0.0994453842186005,1.,-0.809917659739319));
#18722=CARTESIAN_POINT('',(0.0994453842186005,0.,-0.809917659739319));
#18723=CARTESIAN_POINT('',(0.0663886785289726,1.,-0.813294868644317));
#18724=CARTESIAN_POINT('Origin',(2.22044604925031E-16,-1.,-1.07625882986966));
#18725=CARTESIAN_POINT('',(0.163621780455751,-1.,-1.33259246319364));
#18726=CARTESIAN_POINT('',(0.0994453842186005,-1.,-0.809917659739319));
#18727=CARTESIAN_POINT('',(0.0994453842186005,-1.,-0.809917659739319));
#18728=CARTESIAN_POINT('',(0.0663886785289726,-1.,-0.813294868644317));
#18729=CARTESIAN_POINT('',(0.0663886785289726,-1.,-0.813294868644317));
#18730=CARTESIAN_POINT('',(0.0332218842499744,-1.,-0.815323436684413));
#18731=CARTESIAN_POINT('',(0.0332218842499744,-1.,-0.815323436684413));
#18732=CARTESIAN_POINT('',(2.22044604925031E-16,-1.,-0.816));
#18733=CARTESIAN_POINT('',(2.22044604925031E-16,-1.,-0.816));
#18734=CARTESIAN_POINT('',(-0.033221884249974,-1.,-0.815323436684413));
#18735=CARTESIAN_POINT('',(-0.033221884249974,-1.,-0.815323436684413));
#18736=CARTESIAN_POINT('',(-0.0663886785289722,-1.,-0.813294868644317));
#18737=CARTESIAN_POINT('',(-0.109232156609066,-1.,-1.33814913068855));
#18738=CARTESIAN_POINT('',(-0.109232156609066,-1.,-1.33814913068855));
#18739=CARTESIAN_POINT('',(-0.0546613992573715,-1.,-1.34148682119178));
#18740=CARTESIAN_POINT('',(-0.0546613992573715,-1.,-1.34148682119178));
#18741=CARTESIAN_POINT('',(2.22044604925031E-16,-1.,-1.3426));
#18742=CARTESIAN_POINT('',(2.22044604925031E-16,-1.,-1.3426));
#18743=CARTESIAN_POINT('',(0.054661399257372,-1.,-1.34148682119178));
#18744=CARTESIAN_POINT('',(0.054661399257372,-1.,-1.34148682119178));
#18745=CARTESIAN_POINT('',(0.109232156609067,-1.,-1.33814913068855));
#18746=CARTESIAN_POINT('',(0.109232156609067,-1.,-1.33814913068855));
#18747=CARTESIAN_POINT('',(0.163621780455751,-1.,-1.33259246319364));
#18748=CARTESIAN_POINT('Origin',(0.0663886785289726,0.,-0.813294868644317));
#18749=CARTESIAN_POINT('',(0.0663886785289726,0.,-0.813294868644317));
#18750=CARTESIAN_POINT('',(0.0994453842186005,0.,-0.809917659739319));
#18751=CARTESIAN_POINT('Origin',(0.0332218842499744,0.,-0.815323436684413));
#18752=CARTESIAN_POINT('',(0.0332218842499744,0.,-0.815323436684413));
#18753=CARTESIAN_POINT('Origin',(2.22044604925031E-16,0.,-0.816));
#18754=CARTESIAN_POINT('',(2.22044604925031E-16,0.,-0.816));
#18755=CARTESIAN_POINT('Origin',(-0.033221884249974,0.,-0.815323436684413));
#18756=CARTESIAN_POINT('',(-0.033221884249974,0.,-0.815323436684413));
#18757=CARTESIAN_POINT('Origin',(-0.0663886785289722,0.,-0.813294868644317));
#18758=CARTESIAN_POINT('Origin',(-0.109232156609066,0.,-1.33814913068855));
#18759=CARTESIAN_POINT('',(-0.109232156609066,1.,-1.33814913068855));
#18760=CARTESIAN_POINT('',(-0.109232156609066,1.,-1.33814913068855));
#18761=CARTESIAN_POINT('',(-0.109232156609066,0.,-1.33814913068855));
#18762=CARTESIAN_POINT('Origin',(-0.0546613992573715,0.,-1.34148682119178));
#18763=CARTESIAN_POINT('',(-0.0546613992573715,1.,-1.34148682119178));
#18764=CARTESIAN_POINT('',(-0.0546613992573715,1.,-1.34148682119178));
#18765=CARTESIAN_POINT('',(-0.0546613992573715,0.,-1.34148682119178));
#18766=CARTESIAN_POINT('Origin',(2.22044604925031E-16,0.,-1.3426));
#18767=CARTESIAN_POINT('',(2.22044604925031E-16,1.,-1.3426));
#18768=CARTESIAN_POINT('',(2.22044604925031E-16,1.,-1.3426));
#18769=CARTESIAN_POINT('',(2.22044604925031E-16,0.,-1.3426));
#18770=CARTESIAN_POINT('Origin',(0.054661399257372,0.,-1.34148682119178));
#18771=CARTESIAN_POINT('',(0.054661399257372,1.,-1.34148682119178));
#18772=CARTESIAN_POINT('',(0.054661399257372,1.,-1.34148682119178));
#18773=CARTESIAN_POINT('',(0.054661399257372,0.,-1.34148682119178));
#18774=CARTESIAN_POINT('Origin',(0.109232156609067,0.,-1.33814913068855));
#18775=CARTESIAN_POINT('',(0.109232156609067,1.,-1.33814913068855));
#18776=CARTESIAN_POINT('',(0.109232156609067,1.,-1.33814913068855));
#18777=CARTESIAN_POINT('',(0.109232156609067,0.,-1.33814913068855));
#18778=CARTESIAN_POINT('Origin',(0.163621780455751,0.,-1.33259246319364));
#18779=CARTESIAN_POINT('',(0.163621780455751,1.,-1.33259246319364));
#18780=CARTESIAN_POINT('',(0.163621780455751,1.,-1.33259246319364));
#18781=CARTESIAN_POINT('',(0.163621780455751,0.,-1.33259246319364));
#18782=CARTESIAN_POINT('Origin',(0.0994453842186005,0.,-0.809917659739319));
#18783=CARTESIAN_POINT('',(0.0994453842186005,1.,-0.809917659739319));
#18784=CARTESIAN_POINT('Origin',(2.22044604925031E-16,1.,-1.07625882986966));
#18785=CARTESIAN_POINT('Origin',(1.0722480357895,0.,-0.80799685008394));
#18786=CARTESIAN_POINT('',(0.651686576198591,1.,-0.491081058892071));
#18787=CARTESIAN_POINT('',(0.651686576198591,0.,-0.491081058892071));
#18788=CARTESIAN_POINT('',(1.0722480357895,1.,-0.80799685008394));
#18789=CARTESIAN_POINT('',(1.0722480357895,1.,-0.80799685008394));
#18790=CARTESIAN_POINT('',(1.0722480357895,-1.,-0.80799685008394));
#18791=CARTESIAN_POINT('',(1.0722480357895,0.,-0.80799685008394));
#18792=CARTESIAN_POINT('',(0.651686576198591,-1.,-0.491081058892071));
#18793=CARTESIAN_POINT('',(1.0722480357895,-1.,-0.80799685008394));
#18794=CARTESIAN_POINT('',(0.651686576198591,0.,-0.491081058892071));
#18795=CARTESIAN_POINT('Origin',(0.651686576198591,0.,-0.491081058892071));
#18796=CARTESIAN_POINT('',(0.67113967774902,1.,-0.464141716451927));
#18797=CARTESIAN_POINT('',(0.67113967774902,0.,-0.464141716451927));
#18798=CARTESIAN_POINT('',(0.651686576198591,1.,-0.491081058892071));
#18799=CARTESIAN_POINT('Origin',(0.651686576198591,0.,-0.491081058892071));
#18800=CARTESIAN_POINT('',(0.67113967774902,-1.,-0.464141716451927));
#18801=CARTESIAN_POINT('',(0.651686576198591,-1.,-0.491081058892071));
#18802=CARTESIAN_POINT('',(0.67113967774902,0.,-0.464141716451927));
#18803=CARTESIAN_POINT('Origin',(0.67113967774902,0.,-0.464141716451927));
#18804=CARTESIAN_POINT('',(0.689479866344548,1.,-0.43643271406427));
#18805=CARTESIAN_POINT('',(0.689479866344548,0.,-0.43643271406427));
#18806=CARTESIAN_POINT('',(0.67113967774902,1.,-0.464141716451927));
#18807=CARTESIAN_POINT('Origin',(0.689479866344548,0.,-0.43643271406427));
#18808=CARTESIAN_POINT('',(0.706676729488102,1.,-0.408));
#18809=CARTESIAN_POINT('',(0.706676729488102,0.,-0.408));
#18810=CARTESIAN_POINT('',(0.689479866344548,1.,-0.43643271406427));
#18811=CARTESIAN_POINT('Origin',(0.706676729488102,0.,-0.408));
#18812=CARTESIAN_POINT('',(0.722701750594522,1.,-0.378890722620142));
#18813=CARTESIAN_POINT('',(0.722701750594522,0.,-0.378890722620142));
#18814=CARTESIAN_POINT('',(0.706676729488102,1.,-0.408));
#18815=CARTESIAN_POINT('Origin',(0.722701750594522,0.,-0.378890722620142));
#18816=CARTESIAN_POINT('',(0.737528356277993,1.,-0.34915315219239));
#18817=CARTESIAN_POINT('',(0.737528356277993,0.,-0.34915315219239));
#18818=CARTESIAN_POINT('',(0.722701750594522,1.,-0.378890722620142));
#18819=CARTESIAN_POINT('Origin',(0.737528356277993,0.,-0.34915315219239));
#18820=CARTESIAN_POINT('',(0.751131960417191,1.,-0.318836600847247));
#18821=CARTESIAN_POINT('',(0.751131960417191,0.,-0.318836600847247));
#18822=CARTESIAN_POINT('',(0.737528356277993,1.,-0.34915315219239));
#18823=CARTESIAN_POINT('Origin',(0.932067487714439,-1.,-0.53812941493483));
#18824=CARTESIAN_POINT('',(1.23586981624525,-1.,-0.524595613109699));
#18825=CARTESIAN_POINT('',(0.751131960417191,-1.,-0.318836600847247));
#18826=CARTESIAN_POINT('',(0.751131960417191,-1.,-0.318836600847247));
#18827=CARTESIAN_POINT('',(0.737528356277993,-1.,-0.34915315219239));
#18828=CARTESIAN_POINT('',(0.737528356277993,-1.,-0.34915315219239));
#18829=CARTESIAN_POINT('',(0.722701750594522,-1.,-0.378890722620142));
#18830=CARTESIAN_POINT('',(0.722701750594522,-1.,-0.378890722620142));
#18831=CARTESIAN_POINT('',(0.706676729488102,-1.,-0.408));
#18832=CARTESIAN_POINT('',(0.706676729488102,-1.,-0.408));
#18833=CARTESIAN_POINT('',(0.689479866344548,-1.,-0.43643271406427));
#18834=CARTESIAN_POINT('',(0.689479866344548,-1.,-0.43643271406427));
#18835=CARTESIAN_POINT('',(0.67113967774902,-1.,-0.464141716451927));
#18836=CARTESIAN_POINT('',(1.10425506292382,-1.,-0.763672387877889));
#18837=CARTESIAN_POINT('',(1.10425506292382,-1.,-0.763672387877889));
#18838=CARTESIAN_POINT('',(1.13443096636543,-1.,-0.718081570959178));
#18839=CARTESIAN_POINT('',(1.13443096636543,-1.,-0.718081570959177));
#18840=CARTESIAN_POINT('',(1.16272570712099,-1.,-0.6713));
#18841=CARTESIAN_POINT('',(1.16272570712099,-1.,-0.6713));
#18842=CARTESIAN_POINT('',(1.1890923656228,-1.,-0.623405250232602));
#18843=CARTESIAN_POINT('',(1.1890923656228,-1.,-0.623405250232602));
#18844=CARTESIAN_POINT('',(1.21348721953288,-1.,-0.574476742810665));
#18845=CARTESIAN_POINT('',(1.21348721953288,-1.,-0.574476742810665));
#18846=CARTESIAN_POINT('',(1.23586981624525,-1.,-0.524595613109699));
#18847=CARTESIAN_POINT('Origin',(0.737528356277993,0.,-0.34915315219239));
#18848=CARTESIAN_POINT('',(0.737528356277993,0.,-0.34915315219239));
#18849=CARTESIAN_POINT('',(0.751131960417191,0.,-0.318836600847247));
#18850=CARTESIAN_POINT('Origin',(0.722701750594522,0.,-0.378890722620142));
#18851=CARTESIAN_POINT('',(0.722701750594522,0.,-0.378890722620142));
#18852=CARTESIAN_POINT('Origin',(0.706676729488102,0.,-0.408));
#18853=CARTESIAN_POINT('',(0.706676729488102,0.,-0.408));
#18854=CARTESIAN_POINT('Origin',(0.689479866344548,0.,-0.43643271406427));
#18855=CARTESIAN_POINT('',(0.689479866344548,0.,-0.43643271406427));
#18856=CARTESIAN_POINT('Origin',(0.67113967774902,0.,-0.464141716451927));
#18857=CARTESIAN_POINT('Origin',(1.10425506292382,0.,-0.763672387877889));
#18858=CARTESIAN_POINT('',(1.10425506292382,1.,-0.763672387877889));
#18859=CARTESIAN_POINT('',(1.10425506292382,1.,-0.763672387877889));
#18860=CARTESIAN_POINT('',(1.10425506292382,0.,-0.763672387877889));
#18861=CARTESIAN_POINT('Origin',(1.13443096636543,0.,-0.718081570959177));
#18862=CARTESIAN_POINT('',(1.13443096636543,1.,-0.718081570959178));
#18863=CARTESIAN_POINT('',(1.13443096636543,1.,-0.718081570959177));
#18864=CARTESIAN_POINT('',(1.13443096636543,0.,-0.718081570959177));
#18865=CARTESIAN_POINT('Origin',(1.16272570712099,0.,-0.6713));
#18866=CARTESIAN_POINT('',(1.16272570712099,1.,-0.6713));
#18867=CARTESIAN_POINT('',(1.16272570712099,1.,-0.6713));
#18868=CARTESIAN_POINT('',(1.16272570712099,0.,-0.6713));
#18869=CARTESIAN_POINT('Origin',(1.1890923656228,0.,-0.623405250232602));
#18870=CARTESIAN_POINT('',(1.1890923656228,1.,-0.623405250232602));
#18871=CARTESIAN_POINT('',(1.1890923656228,1.,-0.623405250232602));
#18872=CARTESIAN_POINT('',(1.1890923656228,0.,-0.623405250232602));
#18873=CARTESIAN_POINT('Origin',(1.21348721953288,0.,-0.574476742810665));
#18874=CARTESIAN_POINT('',(1.21348721953288,1.,-0.574476742810665));
#18875=CARTESIAN_POINT('',(1.21348721953288,1.,-0.574476742810665));
#18876=CARTESIAN_POINT('',(1.21348721953288,0.,-0.574476742810665));
#18877=CARTESIAN_POINT('Origin',(1.23586981624525,0.,-0.524595613109699));
#18878=CARTESIAN_POINT('',(1.23586981624525,1.,-0.524595613109699));
#18879=CARTESIAN_POINT('',(1.23586981624525,1.,-0.524595613109699));
#18880=CARTESIAN_POINT('',(1.23586981624525,0.,-0.524595613109699));
#18881=CARTESIAN_POINT('Origin',(0.751131960417191,0.,-0.318836600847247));
#18882=CARTESIAN_POINT('',(0.751131960417191,1.,-0.318836600847247));
#18883=CARTESIAN_POINT('Origin',(0.932067487714439,1.,-0.53812941493483));
#18884=CARTESIAN_POINT('Origin',(-1.23586981624525,0.,-0.524595613109699));
#18885=CARTESIAN_POINT('',(-0.751131960417191,1.,-0.318836600847248));
#18886=CARTESIAN_POINT('',(-0.751131960417191,0.,-0.318836600847248));
#18887=CARTESIAN_POINT('',(-1.23586981624525,1.,-0.524595613109699));
#18888=CARTESIAN_POINT('',(-1.23586981624525,1.,-0.524595613109699));
#18889=CARTESIAN_POINT('',(-1.23586981624525,-1.,-0.524595613109699));
#18890=CARTESIAN_POINT('',(-1.23586981624525,0.,-0.524595613109699));
#18891=CARTESIAN_POINT('',(-0.751131960417191,-1.,-0.318836600847248));
#18892=CARTESIAN_POINT('',(-1.23586981624525,-1.,-0.524595613109699));
#18893=CARTESIAN_POINT('',(-0.751131960417191,0.,-0.318836600847248));
#18894=CARTESIAN_POINT('Origin',(-0.751131960417191,0.,-0.318836600847248));
#18895=CARTESIAN_POINT('',(-0.737528356277993,1.,-0.34915315219239));
#18896=CARTESIAN_POINT('',(-0.737528356277993,0.,-0.34915315219239));
#18897=CARTESIAN_POINT('',(-0.751131960417191,1.,-0.318836600847248));
#18898=CARTESIAN_POINT('Origin',(-0.751131960417191,0.,-0.318836600847248));
#18899=CARTESIAN_POINT('',(-0.737528356277993,-1.,-0.34915315219239));
#18900=CARTESIAN_POINT('',(-0.751131960417191,-1.,-0.318836600847248));
#18901=CARTESIAN_POINT('',(-0.737528356277993,0.,-0.34915315219239));
#18902=CARTESIAN_POINT('Origin',(-0.737528356277993,0.,-0.34915315219239));
#18903=CARTESIAN_POINT('',(-0.722701750594522,1.,-0.378890722620143));
#18904=CARTESIAN_POINT('',(-0.722701750594522,0.,-0.378890722620143));
#18905=CARTESIAN_POINT('',(-0.737528356277993,1.,-0.34915315219239));
#18906=CARTESIAN_POINT('Origin',(-0.722701750594522,0.,-0.378890722620143));
#18907=CARTESIAN_POINT('',(-0.706676729488102,1.,-0.408));
#18908=CARTESIAN_POINT('',(-0.706676729488102,0.,-0.408));
#18909=CARTESIAN_POINT('',(-0.722701750594522,1.,-0.378890722620143));
#18910=CARTESIAN_POINT('Origin',(-0.706676729488102,0.,-0.408));
#18911=CARTESIAN_POINT('',(-0.689479866344548,1.,-0.43643271406427));
#18912=CARTESIAN_POINT('',(-0.689479866344548,0.,-0.43643271406427));
#18913=CARTESIAN_POINT('',(-0.706676729488102,1.,-0.408));
#18914=CARTESIAN_POINT('Origin',(-0.689479866344548,0.,-0.43643271406427));
#18915=CARTESIAN_POINT('',(-0.67113967774902,1.,-0.464141716451927));
#18916=CARTESIAN_POINT('',(-0.67113967774902,0.,-0.464141716451927));
#18917=CARTESIAN_POINT('',(-0.689479866344548,1.,-0.43643271406427));
#18918=CARTESIAN_POINT('Origin',(-0.67113967774902,0.,-0.464141716451927));
#18919=CARTESIAN_POINT('',(-0.651686576198591,1.,-0.491081058892072));
#18920=CARTESIAN_POINT('',(-0.651686576198591,0.,-0.491081058892072));
#18921=CARTESIAN_POINT('',(-0.67113967774902,1.,-0.464141716451927));
#18922=CARTESIAN_POINT('Origin',(-0.932067487714439,-1.,-0.53812941493483));
#18923=CARTESIAN_POINT('',(-1.0722480357895,-1.,-0.80799685008394));
#18924=CARTESIAN_POINT('',(-0.651686576198591,-1.,-0.491081058892072));
#18925=CARTESIAN_POINT('',(-0.651686576198591,-1.,-0.491081058892072));
#18926=CARTESIAN_POINT('',(-0.67113967774902,-1.,-0.464141716451927));
#18927=CARTESIAN_POINT('',(-0.67113967774902,-1.,-0.464141716451927));
#18928=CARTESIAN_POINT('',(-0.689479866344548,-1.,-0.43643271406427));
#18929=CARTESIAN_POINT('',(-0.689479866344548,-1.,-0.43643271406427));
#18930=CARTESIAN_POINT('',(-0.706676729488102,-1.,-0.408));
#18931=CARTESIAN_POINT('',(-0.706676729488102,-1.,-0.408));
#18932=CARTESIAN_POINT('',(-0.722701750594522,-1.,-0.378890722620143));
#18933=CARTESIAN_POINT('',(-0.722701750594522,-1.,-0.378890722620143));
#18934=CARTESIAN_POINT('',(-0.737528356277993,-1.,-0.34915315219239));
#18935=CARTESIAN_POINT('',(-1.21348721953288,-1.,-0.574476742810665));
#18936=CARTESIAN_POINT('',(-1.21348721953288,-1.,-0.574476742810665));
#18937=CARTESIAN_POINT('',(-1.1890923656228,-1.,-0.623405250232602));
#18938=CARTESIAN_POINT('',(-1.1890923656228,-1.,-0.623405250232602));
#18939=CARTESIAN_POINT('',(-1.16272570712099,-1.,-0.6713));
#18940=CARTESIAN_POINT('',(-1.16272570712099,-1.,-0.6713));
#18941=CARTESIAN_POINT('',(-1.13443096636543,-1.,-0.718081570959178));
#18942=CARTESIAN_POINT('',(-1.13443096636543,-1.,-0.718081570959178));
#18943=CARTESIAN_POINT('',(-1.10425506292382,-1.,-0.763672387877889));
#18944=CARTESIAN_POINT('',(-1.10425506292382,-1.,-0.763672387877889));
#18945=CARTESIAN_POINT('',(-1.0722480357895,-1.,-0.80799685008394));
#18946=CARTESIAN_POINT('Origin',(-0.67113967774902,0.,-0.464141716451927));
#18947=CARTESIAN_POINT('',(-0.67113967774902,0.,-0.464141716451927));
#18948=CARTESIAN_POINT('',(-0.651686576198591,0.,-0.491081058892072));
#18949=CARTESIAN_POINT('Origin',(-0.689479866344548,0.,-0.43643271406427));
#18950=CARTESIAN_POINT('',(-0.689479866344548,0.,-0.43643271406427));
#18951=CARTESIAN_POINT('Origin',(-0.706676729488102,0.,-0.408));
#18952=CARTESIAN_POINT('',(-0.706676729488102,0.,-0.408));
#18953=CARTESIAN_POINT('Origin',(-0.722701750594522,0.,-0.378890722620143));
#18954=CARTESIAN_POINT('',(-0.722701750594522,0.,-0.378890722620143));
#18955=CARTESIAN_POINT('Origin',(-0.737528356277993,0.,-0.34915315219239));
#18956=CARTESIAN_POINT('Origin',(-1.21348721953288,0.,-0.574476742810665));
#18957=CARTESIAN_POINT('',(-1.21348721953288,1.,-0.574476742810665));
#18958=CARTESIAN_POINT('',(-1.21348721953288,1.,-0.574476742810665));
#18959=CARTESIAN_POINT('',(-1.21348721953288,0.,-0.574476742810665));
#18960=CARTESIAN_POINT('Origin',(-1.1890923656228,0.,-0.623405250232602));
#18961=CARTESIAN_POINT('',(-1.1890923656228,1.,-0.623405250232602));
#18962=CARTESIAN_POINT('',(-1.1890923656228,1.,-0.623405250232602));
#18963=CARTESIAN_POINT('',(-1.1890923656228,0.,-0.623405250232602));
#18964=CARTESIAN_POINT('Origin',(-1.16272570712099,0.,-0.6713));
#18965=CARTESIAN_POINT('',(-1.16272570712099,1.,-0.6713));
#18966=CARTESIAN_POINT('',(-1.16272570712099,1.,-0.6713));
#18967=CARTESIAN_POINT('',(-1.16272570712099,0.,-0.6713));
#18968=CARTESIAN_POINT('Origin',(-1.13443096636543,0.,-0.718081570959178));
#18969=CARTESIAN_POINT('',(-1.13443096636543,1.,-0.718081570959178));
#18970=CARTESIAN_POINT('',(-1.13443096636543,1.,-0.718081570959178));
#18971=CARTESIAN_POINT('',(-1.13443096636543,0.,-0.718081570959178));
#18972=CARTESIAN_POINT('Origin',(-1.10425506292382,0.,-0.763672387877889));
#18973=CARTESIAN_POINT('',(-1.10425506292382,1.,-0.763672387877889));
#18974=CARTESIAN_POINT('',(-1.10425506292382,1.,-0.763672387877889));
#18975=CARTESIAN_POINT('',(-1.10425506292382,0.,-0.763672387877889));
#18976=CARTESIAN_POINT('Origin',(-1.0722480357895,0.,-0.80799685008394));
#18977=CARTESIAN_POINT('',(-1.0722480357895,1.,-0.80799685008394));
#18978=CARTESIAN_POINT('',(-1.0722480357895,1.,-0.80799685008394));
#18979=CARTESIAN_POINT('',(-1.0722480357895,0.,-0.80799685008394));
#18980=CARTESIAN_POINT('Origin',(-0.651686576198591,0.,-0.491081058892072));
#18981=CARTESIAN_POINT('',(-0.651686576198591,1.,-0.491081058892072));
#18982=CARTESIAN_POINT('Origin',(-0.932067487714439,1.,-0.53812941493483));
#18983=CARTESIAN_POINT('Origin',(0.16362178045575,0.,1.33259246319364));
#18984=CARTESIAN_POINT('',(0.0994453842185998,1.,0.809917659739319));
#18985=CARTESIAN_POINT('',(0.0994453842185998,0.,0.809917659739319));
#18986=CARTESIAN_POINT('',(0.16362178045575,1.,1.33259246319364));
#18987=CARTESIAN_POINT('',(0.16362178045575,1.,1.33259246319364));
#18988=CARTESIAN_POINT('',(0.16362178045575,-1.,1.33259246319364));
#18989=CARTESIAN_POINT('',(0.16362178045575,0.,1.33259246319364));
#18990=CARTESIAN_POINT('',(0.0994453842185998,-1.,0.809917659739319));
#18991=CARTESIAN_POINT('',(0.16362178045575,-1.,1.33259246319364));
#18992=CARTESIAN_POINT('',(0.0994453842185998,0.,0.809917659739319));
#18993=CARTESIAN_POINT('Origin',(0.0994453842185998,0.,0.809917659739319));
#18994=CARTESIAN_POINT('',(0.0663886785289718,1.,0.813294868644317));
#18995=CARTESIAN_POINT('',(0.0663886785289718,0.,0.813294868644317));
#18996=CARTESIAN_POINT('',(0.0994453842185998,1.,0.809917659739319));
#18997=CARTESIAN_POINT('Origin',(0.0994453842185998,0.,0.809917659739319));
#18998=CARTESIAN_POINT('',(0.0663886785289718,-1.,0.813294868644317));
#18999=CARTESIAN_POINT('',(0.0994453842185998,-1.,0.809917659739319));
#19000=CARTESIAN_POINT('',(0.0663886785289718,0.,0.813294868644317));
#19001=CARTESIAN_POINT('Origin',(0.0663886785289718,0.,0.813294868644317));
#19002=CARTESIAN_POINT('',(0.0332218842499737,1.,0.815323436684413));
#19003=CARTESIAN_POINT('',(0.0332218842499737,0.,0.815323436684413));
#19004=CARTESIAN_POINT('',(0.0663886785289718,1.,0.813294868644317));
#19005=CARTESIAN_POINT('Origin',(0.0332218842499737,0.,0.815323436684413));
#19006=CARTESIAN_POINT('',(-4.9960036108132E-16,1.,0.816));
#19007=CARTESIAN_POINT('',(-4.9960036108132E-16,0.,0.816));
#19008=CARTESIAN_POINT('',(0.0332218842499737,1.,0.815323436684413));
#19009=CARTESIAN_POINT('Origin',(-4.9960036108132E-16,0.,0.816));
#19010=CARTESIAN_POINT('',(-0.0332218842499747,1.,0.815323436684413));
#19011=CARTESIAN_POINT('',(-0.0332218842499747,0.,0.815323436684413));
#19012=CARTESIAN_POINT('',(-4.9960036108132E-16,1.,0.816));
#19013=CARTESIAN_POINT('Origin',(-0.0332218842499747,0.,0.815323436684413));
#19014=CARTESIAN_POINT('',(-0.0663886785289729,1.,0.813294868644317));
#19015=CARTESIAN_POINT('',(-0.0663886785289729,0.,0.813294868644317));
#19016=CARTESIAN_POINT('',(-0.0332218842499747,1.,0.815323436684413));
#19017=CARTESIAN_POINT('Origin',(-0.0663886785289729,0.,0.813294868644317));
#19018=CARTESIAN_POINT('',(-0.0994453842186008,1.,0.809917659739319));
#19019=CARTESIAN_POINT('',(-0.0994453842186008,0.,0.809917659739319));
#19020=CARTESIAN_POINT('',(-0.0663886785289729,1.,0.813294868644317));
#19021=CARTESIAN_POINT('Origin',(-6.10622663543836E-16,-1.,1.07625882986966));
#19022=CARTESIAN_POINT('',(-0.163621780455752,-1.,1.33259246319364));
#19023=CARTESIAN_POINT('',(-0.0994453842186008,-1.,0.809917659739319));
#19024=CARTESIAN_POINT('',(-0.0994453842186008,-1.,0.809917659739319));
#19025=CARTESIAN_POINT('',(-0.0663886785289729,-1.,0.813294868644317));
#19026=CARTESIAN_POINT('',(-0.0663886785289729,-1.,0.813294868644317));
#19027=CARTESIAN_POINT('',(-0.0332218842499747,-1.,0.815323436684413));
#19028=CARTESIAN_POINT('',(-0.0332218842499747,-1.,0.815323436684413));
#19029=CARTESIAN_POINT('',(-4.9960036108132E-16,-1.,0.816));
#19030=CARTESIAN_POINT('',(-4.9960036108132E-16,-1.,0.816));
#19031=CARTESIAN_POINT('',(0.0332218842499737,-1.,0.815323436684413));
#19032=CARTESIAN_POINT('',(0.0332218842499737,-1.,0.815323436684413));
#19033=CARTESIAN_POINT('',(0.0663886785289718,-1.,0.813294868644317));
#19034=CARTESIAN_POINT('',(0.109232156609066,-1.,1.33814913068855));
#19035=CARTESIAN_POINT('',(0.109232156609066,-1.,1.33814913068855));
#19036=CARTESIAN_POINT('',(0.054661399257371,-1.,1.34148682119178));
#19037=CARTESIAN_POINT('',(0.054661399257371,-1.,1.34148682119178));
#19038=CARTESIAN_POINT('',(-7.7715611723761E-16,-1.,1.3426));
#19039=CARTESIAN_POINT('',(-7.7715611723761E-16,-1.,1.3426));
#19040=CARTESIAN_POINT('',(-0.0546613992573726,-1.,1.34148682119178));
#19041=CARTESIAN_POINT('',(-0.0546613992573726,-1.,1.34148682119178));
#19042=CARTESIAN_POINT('',(-0.109232156609067,-1.,1.33814913068855));
#19043=CARTESIAN_POINT('',(-0.109232156609067,-1.,1.33814913068855));
#19044=CARTESIAN_POINT('',(-0.163621780455752,-1.,1.33259246319364));
#19045=CARTESIAN_POINT('Origin',(-0.0663886785289729,0.,0.813294868644317));
#19046=CARTESIAN_POINT('',(-0.0663886785289729,0.,0.813294868644317));
#19047=CARTESIAN_POINT('',(-0.0994453842186008,0.,0.809917659739319));
#19048=CARTESIAN_POINT('Origin',(-0.0332218842499747,0.,0.815323436684413));
#19049=CARTESIAN_POINT('',(-0.0332218842499747,0.,0.815323436684413));
#19050=CARTESIAN_POINT('Origin',(-4.9960036108132E-16,0.,0.816));
#19051=CARTESIAN_POINT('',(-4.9960036108132E-16,0.,0.816));
#19052=CARTESIAN_POINT('Origin',(0.0332218842499737,0.,0.815323436684413));
#19053=CARTESIAN_POINT('',(0.0332218842499737,0.,0.815323436684413));
#19054=CARTESIAN_POINT('Origin',(0.0663886785289718,0.,0.813294868644317));
#19055=CARTESIAN_POINT('Origin',(0.109232156609066,0.,1.33814913068855));
#19056=CARTESIAN_POINT('',(0.109232156609066,1.,1.33814913068855));
#19057=CARTESIAN_POINT('',(0.109232156609066,1.,1.33814913068855));
#19058=CARTESIAN_POINT('',(0.109232156609066,0.,1.33814913068855));
#19059=CARTESIAN_POINT('Origin',(0.054661399257371,0.,1.34148682119178));
#19060=CARTESIAN_POINT('',(0.054661399257371,1.,1.34148682119178));
#19061=CARTESIAN_POINT('',(0.054661399257371,1.,1.34148682119178));
#19062=CARTESIAN_POINT('',(0.054661399257371,0.,1.34148682119178));
#19063=CARTESIAN_POINT('Origin',(-7.7715611723761E-16,0.,1.3426));
#19064=CARTESIAN_POINT('',(-7.7715611723761E-16,1.,1.3426));
#19065=CARTESIAN_POINT('',(-7.7715611723761E-16,1.,1.3426));
#19066=CARTESIAN_POINT('',(-7.7715611723761E-16,0.,1.3426));
#19067=CARTESIAN_POINT('Origin',(-0.0546613992573726,0.,1.34148682119178));
#19068=CARTESIAN_POINT('',(-0.0546613992573726,1.,1.34148682119178));
#19069=CARTESIAN_POINT('',(-0.0546613992573726,1.,1.34148682119178));
#19070=CARTESIAN_POINT('',(-0.0546613992573726,0.,1.34148682119178));
#19071=CARTESIAN_POINT('Origin',(-0.109232156609067,0.,1.33814913068855));
#19072=CARTESIAN_POINT('',(-0.109232156609067,1.,1.33814913068855));
#19073=CARTESIAN_POINT('',(-0.109232156609067,1.,1.33814913068855));
#19074=CARTESIAN_POINT('',(-0.109232156609067,0.,1.33814913068855));
#19075=CARTESIAN_POINT('Origin',(-0.163621780455752,0.,1.33259246319364));
#19076=CARTESIAN_POINT('',(-0.163621780455752,1.,1.33259246319364));
#19077=CARTESIAN_POINT('',(-0.163621780455752,1.,1.33259246319364));
#19078=CARTESIAN_POINT('',(-0.163621780455752,0.,1.33259246319364));
#19079=CARTESIAN_POINT('Origin',(-0.0994453842186008,0.,0.809917659739319));
#19080=CARTESIAN_POINT('',(-0.0994453842186008,1.,0.809917659739319));
#19081=CARTESIAN_POINT('Origin',(-6.10622663543836E-16,1.,1.07625882986966));
#19082=CARTESIAN_POINT('',(0.,0.,0.));
#19083=CARTESIAN_POINT('',(0.,0.,0.));
#19084=CARTESIAN_POINT('',(0.,0.,0.));
#19085=CARTESIAN_POINT('',(0.,0.,0.));
#19086=CARTESIAN_POINT('Origin',(0.4,0.18,0.38));
#19087=CARTESIAN_POINT('',(-0.8,0.2,0.36));
#19088=CARTESIAN_POINT('',(-0.8,0.16,0.4));
#19089=CARTESIAN_POINT('',(-0.8,0.2,0.36));
#19090=CARTESIAN_POINT('',(0.8,0.16,0.4));
#19091=CARTESIAN_POINT('',(0.4,0.16,0.4));
#19092=CARTESIAN_POINT('',(0.8,0.2,0.36));
#19093=CARTESIAN_POINT('',(0.8,0.16,0.4));
#19094=CARTESIAN_POINT('',(0.4,0.2,0.36));
#19095=CARTESIAN_POINT('Origin',(-0.8,0.,0.38));
#19096=CARTESIAN_POINT('',(-0.8,-0.2,0.36));
#19097=CARTESIAN_POINT('',(-0.8,-0.16,0.4));
#19098=CARTESIAN_POINT('',(-0.8,-0.2,0.36));
#19099=CARTESIAN_POINT('Origin',(-0.8,0.,0.4));
#19100=CARTESIAN_POINT('Origin',(-0.8,0.,0.36));
#19101=CARTESIAN_POINT('Origin',(-0.4,-0.18,0.38));
#19102=CARTESIAN_POINT('',(0.8,-0.2,0.36));
#19103=CARTESIAN_POINT('',(0.8,-0.16,0.4));
#19104=CARTESIAN_POINT('',(0.8,-0.2,0.36));
#19105=CARTESIAN_POINT('',(-0.4,-0.16,0.4));
#19106=CARTESIAN_POINT('',(-0.4,-0.2,0.36));
#19107=CARTESIAN_POINT('Origin',(0.8,0.,0.38));
#19108=CARTESIAN_POINT('Origin',(0.8,0.,0.4));
#19109=CARTESIAN_POINT('Origin',(0.8,0.,0.36));
#19110=CARTESIAN_POINT('Origin',(-0.8,0.,0.));
#19111=CARTESIAN_POINT('',(-0.8,0.2,0.04));
#19112=CARTESIAN_POINT('',(-0.8,0.2,0.));
#19113=CARTESIAN_POINT('',(-0.8,-0.2,0.04));
#19114=CARTESIAN_POINT('Origin',(-0.8,0.,0.04));
#19115=CARTESIAN_POINT('',(-0.8,-0.2,0.));
#19116=CARTESIAN_POINT('Origin',(0.8,0.2,0.));
#19117=CARTESIAN_POINT('',(0.8,0.2,0.04));
#19118=CARTESIAN_POINT('',(0.8,0.2,0.));
#19119=CARTESIAN_POINT('',(0.4,0.2,0.04));
#19120=CARTESIAN_POINT('Origin',(0.,0.,0.4));
#19121=CARTESIAN_POINT('Origin',(0.4,0.18,0.02));
#19122=CARTESIAN_POINT('',(-0.8,0.16,0.));
#19123=CARTESIAN_POINT('',(-0.8,0.16,0.));
#19124=CARTESIAN_POINT('',(0.8,0.16,0.));
#19125=CARTESIAN_POINT('',(0.8,0.2,0.04));
#19126=CARTESIAN_POINT('',(0.4,0.16,0.));
#19127=CARTESIAN_POINT('Origin',(-0.8,0.,0.02));
#19128=CARTESIAN_POINT('',(-0.8,-0.16,0.));
#19129=CARTESIAN_POINT('',(-0.8,-0.16,0.));
#19130=CARTESIAN_POINT('Origin',(-0.8,0.,0.));
#19131=CARTESIAN_POINT('Origin',(-0.4,-0.18,0.02));
#19132=CARTESIAN_POINT('',(0.8,-0.16,0.));
#19133=CARTESIAN_POINT('',(0.8,-0.2,0.04));
#19134=CARTESIAN_POINT('',(0.8,-0.16,0.));
#19135=CARTESIAN_POINT('',(-0.4,-0.2,0.04));
#19136=CARTESIAN_POINT('',(-0.4,-0.16,0.));
#19137=CARTESIAN_POINT('Origin',(0.8,0.,0.02));
#19138=CARTESIAN_POINT('Origin',(0.8,0.,0.04));
#19139=CARTESIAN_POINT('Origin',(0.8,0.,0.));
#19140=CARTESIAN_POINT('Origin',(0.8,0.,0.));
#19141=CARTESIAN_POINT('',(0.8,-0.2,0.));
#19142=CARTESIAN_POINT('Origin',(0.,0.,0.));
#19143=CARTESIAN_POINT('Origin',(-0.8,-0.2,0.));
#19144=CARTESIAN_POINT('',(0.,0.,0.));
#19145=CARTESIAN_POINT('Origin',(0.0721687836487032,0.,-0.125));
#19146=CARTESIAN_POINT('',(0.0721687836487032,0.,-0.125));
#19147=CARTESIAN_POINT('',(0.144337567297406,0.,0.));
#19148=CARTESIAN_POINT('',(0.117710979560879,0.,-0.0461186027918559));
#19149=CARTESIAN_POINT('',(0.0721687836487032,-0.25,-0.125));
#19150=CARTESIAN_POINT('',(0.0721687836487032,0.,-0.125));
#19151=CARTESIAN_POINT('',(0.144337567297406,-0.25,0.));
#19152=CARTESIAN_POINT('',(0.144337567297406,-0.25,0.));
#19153=CARTESIAN_POINT('',(0.144337567297406,0.,0.));
#19154=CARTESIAN_POINT('Origin',(-0.0721687836487032,0.,-0.125));
#19155=CARTESIAN_POINT('',(-0.0721687836487032,0.,-0.125));
#19156=CARTESIAN_POINT('',(0.0739156081756484,0.,-0.125));
#19157=CARTESIAN_POINT('',(-0.0721687836487032,-0.25,-0.125));
#19158=CARTESIAN_POINT('',(-0.0721687836487032,0.,-0.125));
#19159=CARTESIAN_POINT('',(0.0721687836487032,-0.25,-0.125));
#19160=CARTESIAN_POINT('Origin',(-0.144337567297406,0.,-4.16333634234434E-17));
#19161=CARTESIAN_POINT('',(-0.144337567297406,0.,-1.76762539787485E-17));
#19162=CARTESIAN_POINT('',(-0.0987953713852306,0.,-0.0788813972081442));
#19163=CARTESIAN_POINT('',(-0.144337567297406,-0.25,-2.77555756156289E-17));
#19164=CARTESIAN_POINT('',(-0.144337567297406,0.,-1.76762539787485E-17));
#19165=CARTESIAN_POINT('',(-0.0721687836487032,-0.25,-0.125));
#19166=CARTESIAN_POINT('Origin',(-0.0721687836487033,0.,0.125));
#19167=CARTESIAN_POINT('',(-0.0721687836487033,0.,0.125));
#19168=CARTESIAN_POINT('',(-0.0627109795608791,0.,0.141381397208144));
#19169=CARTESIAN_POINT('',(-0.0721687836487033,-0.25,0.125));
#19170=CARTESIAN_POINT('',(-0.0721687836487033,0.,0.125));
#19171=CARTESIAN_POINT('',(-0.144337567297406,-0.25,-1.76762539787485E-17));
#19172=CARTESIAN_POINT('Origin',(0.0721687836487032,0.,0.125));
#19173=CARTESIAN_POINT('',(0.0721687836487032,0.,0.125));
#19174=CARTESIAN_POINT('',(0.146084391824352,0.,0.125));
#19175=CARTESIAN_POINT('',(0.0721687836487032,-0.25,0.125));
#19176=CARTESIAN_POINT('',(0.0721687836487032,0.,0.125));
#19177=CARTESIAN_POINT('',(-0.0721687836487033,-0.25,0.125));
#19178=CARTESIAN_POINT('Origin',(0.144337567297406,0.,0.));
#19179=CARTESIAN_POINT('',(0.153795371385231,0.,-0.0163813972081441));
#19180=CARTESIAN_POINT('',(0.0721687836487032,-0.25,0.125));
#19181=CARTESIAN_POINT('Origin',(0.,-0.25,0.));
#19182=CARTESIAN_POINT('Origin',(0.22,0.,0.));
#19183=CARTESIAN_POINT('',(-0.22,-8.67361737988404E-18,-2.69422295812418E-17));
#19184=CARTESIAN_POINT('Origin',(0.,0.,0.));
#19185=CARTESIAN_POINT('Origin',(0.,-0.015,0.));
#19186=CARTESIAN_POINT('',(-0.24505,-0.02505,-3.00099698131059E-17));
#19187=CARTESIAN_POINT('Origin',(0.,-0.02505,0.));
#19188=CARTESIAN_POINT('',(-0.235,-0.015,-2.87791997799628E-17));
#19189=CARTESIAN_POINT('Origin',(0.,-0.3775,0.));
#19190=CARTESIAN_POINT('',(-0.24505,-0.72995,3.00099698131059E-17));
#19191=CARTESIAN_POINT('Origin',(0.,-0.72995,0.));
#19192=CARTESIAN_POINT('',(-0.24505,-0.3775,-3.00099698131059E-17));
#19193=CARTESIAN_POINT('Origin',(0.,-0.7625,0.));
#19194=CARTESIAN_POINT('',(-0.175,-0.8,-2.14313189850787E-17));
#19195=CARTESIAN_POINT('Origin',(0.,-0.8,0.));
#19196=CARTESIAN_POINT('',(-0.2125,-0.7625,-2.60237444818813E-17));
#19197=CARTESIAN_POINT('Origin',(0.,-0.8,0.));
#19198=CARTESIAN_POINT('',(0.,0.,0.));
#19199=CARTESIAN_POINT('Origin',(0.3,0.4,0.));
#19200=CARTESIAN_POINT('',(-0.3,0.4,-3.67394039744206E-17));
#19201=CARTESIAN_POINT('Origin',(0.,0.4,0.));
#19202=CARTESIAN_POINT('Origin',(0.,0.375,0.));
#19203=CARTESIAN_POINT('',(-0.35,0.35,-4.28626379701573E-17));
#19204=CARTESIAN_POINT('Origin',(0.,0.35,0.));
#19205=CARTESIAN_POINT('',(-0.325,0.375,-3.9801020972289E-17));
#19206=CARTESIAN_POINT('Origin',(0.,0.19,0.));
#19207=CARTESIAN_POINT('',(-0.35,0.03,-4.28626379701574E-17));
#19208=CARTESIAN_POINT('Origin',(0.,0.03,0.));
#19209=CARTESIAN_POINT('',(-0.35,0.19,-4.28626379701574E-17));
#19210=CARTESIAN_POINT('Origin',(0.,0.0149999999999999,0.));
#19211=CARTESIAN_POINT('',(-0.32,-3.29597460435593E-17,-3.91886975727153E-17));
#19212=CARTESIAN_POINT('Origin',(0.,0.,0.));
#19213=CARTESIAN_POINT('',(-0.335,0.0149999999999999,-4.10256677714363E-17));
#19214=CARTESIAN_POINT('Origin',(0.22,0.,0.));
#19215=CARTESIAN_POINT('',(-0.22,-6.93889390390723E-18,-2.69422295812418E-17));
#19216=CARTESIAN_POINT('Origin',(0.,0.,0.));
#19217=CARTESIAN_POINT('Origin',(0.,-0.02,0.));
#19218=CARTESIAN_POINT('',(-0.1954,-0.0492,2.39295984553393E-17));
#19219=CARTESIAN_POINT('Origin',(0.,-0.0492,0.));
#19220=CARTESIAN_POINT('',(-0.21,-0.02,-2.57175827820944E-17));
#19221=CARTESIAN_POINT('Origin',(0.,-0.8,0.));
#19222=CARTESIAN_POINT('',(-0.1954,-1.5646,2.39295984553393E-17));
#19223=CARTESIAN_POINT('Origin',(0.,-1.5646,0.));
#19224=CARTESIAN_POINT('',(-0.1954,-0.8,-2.39295984553393E-17));
#19225=CARTESIAN_POINT('Origin',(0.,-1.58,0.));
#19226=CARTESIAN_POINT('',(-0.16,-1.6,-1.95943487863577E-17));
#19227=CARTESIAN_POINT('Origin',(0.,-1.6,0.));
#19228=CARTESIAN_POINT('',(-0.18,-1.58,-2.20436423846524E-17));
#19229=CARTESIAN_POINT('Origin',(0.,-1.6,0.));
#19230=CARTESIAN_POINT('Origin',(0.0866025403784439,-0.4,-0.15));
#19231=CARTESIAN_POINT('',(0.173205080756888,-0.4,0.));
#19232=CARTESIAN_POINT('',(0.0866025403784439,-0.4,-0.15));
#19233=CARTESIAN_POINT('',(0.173205080756888,-0.4,0.));
#19234=CARTESIAN_POINT('',(0.0866025403784439,-0.64,-0.15));
#19235=CARTESIAN_POINT('',(0.0866025403784439,-0.4,-0.15));
#19236=CARTESIAN_POINT('',(0.173205080756888,-0.64,0.));
#19237=CARTESIAN_POINT('',(0.173205080756888,-0.64,0.));
#19238=CARTESIAN_POINT('',(0.173205080756888,-0.4,0.));
#19239=CARTESIAN_POINT('Origin',(-0.0866025403784438,-0.4,-0.15));
#19240=CARTESIAN_POINT('',(-0.0866025403784438,-0.4,-0.15));
#19241=CARTESIAN_POINT('',(0.0866025403784439,-0.4,-0.15));
#19242=CARTESIAN_POINT('',(-0.0866025403784438,-0.64,-0.15));
#19243=CARTESIAN_POINT('',(-0.0866025403784438,-0.4,-0.15));
#19244=CARTESIAN_POINT('',(0.0866025403784439,-0.64,-0.15));
#19245=CARTESIAN_POINT('Origin',(-0.173205080756888,-0.4,-2.77555756156289E-17));
#19246=CARTESIAN_POINT('',(-0.173205080756888,-0.4,-2.12115047744981E-17));
#19247=CARTESIAN_POINT('',(-0.0866025403784438,-0.4,-0.15));
#19248=CARTESIAN_POINT('',(-0.173205080756888,-0.64,-2.77555756156289E-17));
#19249=CARTESIAN_POINT('',(-0.173205080756888,-0.4,-2.12115047744981E-17));
#19250=CARTESIAN_POINT('',(-0.0866025403784438,-0.64,-0.15));
#19251=CARTESIAN_POINT('Origin',(-0.0866025403784439,-0.4,0.15));
#19252=CARTESIAN_POINT('',(-0.0866025403784439,-0.4,0.15));
#19253=CARTESIAN_POINT('',(-0.173205080756888,-0.4,-2.12115047744981E-17));
#19254=CARTESIAN_POINT('',(-0.0866025403784439,-0.64,0.15));
#19255=CARTESIAN_POINT('',(-0.0866025403784439,-0.4,0.15));
#19256=CARTESIAN_POINT('',(-0.173205080756888,-0.64,-2.12115047744981E-17));
#19257=CARTESIAN_POINT('Origin',(0.0866025403784439,-0.4,0.15));
#19258=CARTESIAN_POINT('',(0.0866025403784439,-0.4,0.15));
#19259=CARTESIAN_POINT('',(-0.0866025403784439,-0.4,0.15));
#19260=CARTESIAN_POINT('',(0.0866025403784439,-0.64,0.15));
#19261=CARTESIAN_POINT('',(0.0866025403784439,-0.4,0.15));
#19262=CARTESIAN_POINT('',(-0.0866025403784439,-0.64,0.15));
#19263=CARTESIAN_POINT('Origin',(0.173205080756888,-0.4,0.));
#19264=CARTESIAN_POINT('',(0.0866025403784439,-0.4,0.15));
#19265=CARTESIAN_POINT('',(0.0866025403784439,-0.64,0.15));
#19266=CARTESIAN_POINT('Origin',(0.,-0.4,-2.77555756156289E-17));
#19267=CARTESIAN_POINT('Origin',(0.,-0.64,-2.77555756156289E-17));
#19268=CARTESIAN_POINT('',(0.,0.,0.));
#19269=CARTESIAN_POINT('',(0.,0.,0.));
#19270=CARTESIAN_POINT('',(0.,0.,0.));
#19271=CARTESIAN_POINT('',(0.,0.,0.));
#19272=CARTESIAN_POINT('',(0.,0.,0.));
#19273=CARTESIAN_POINT('',(0.,0.,0.));
#19274=CARTESIAN_POINT('',(0.,0.,0.));
#19275=CARTESIAN_POINT('',(0.,-5.8,5.07));
#19276=CARTESIAN_POINT('',(0.,-3.5,4.22));
#19277=CARTESIAN_POINT('',(0.,-5.025,5.62));
#19278=CARTESIAN_POINT('',(1.21243556529821,-1.975,4.92));
#19279=CARTESIAN_POINT('',(0.,10.5,3.87));
#19280=CARTESIAN_POINT('',(0.,9.5,5.62));
#19281=CARTESIAN_POINT('',(0.,0.75,5.62));
#19282=CARTESIAN_POINT('',(0.,20.85,5.62));
#19283=CARTESIAN_POINT('',(0.,22.2,4.22));
#19284=CARTESIAN_POINT('',(0.,0.,0.));
#19285=CARTESIAN_POINT('',(0.,0.,0.));
#19286=UNCERTAINTY_MEASURE_WITH_UNIT(LENGTH_MEASURE(0.001),#19362,
'DISTANCE_ACCURACY_VALUE',
'Maximum model space distance between geometric entities at asserted c
onnectivities');
#19287=UNCERTAINTY_MEASURE_WITH_UNIT(LENGTH_MEASURE(0.001),#19362,
'DISTANCE_ACCURACY_VALUE',
'Maximum model space distance between geometric entities at asserted c
onnectivities');
#19288=UNCERTAINTY_MEASURE_WITH_UNIT(LENGTH_MEASURE(0.001),#19362,
'DISTANCE_ACCURACY_VALUE',
'Maximum model space distance between geometric entities at asserted c
onnectivities');
#19289=UNCERTAINTY_MEASURE_WITH_UNIT(LENGTH_MEASURE(0.001),#19362,
'DISTANCE_ACCURACY_VALUE',
'Maximum model space distance between geometric entities at asserted c
onnectivities');
#19290=UNCERTAINTY_MEASURE_WITH_UNIT(LENGTH_MEASURE(0.001),#19362,
'DISTANCE_ACCURACY_VALUE',
'Maximum model space distance between geometric entities at asserted c
onnectivities');
#19291=UNCERTAINTY_MEASURE_WITH_UNIT(LENGTH_MEASURE(0.001),#19362,
'DISTANCE_ACCURACY_VALUE',
'Maximum model space distance between geometric entities at asserted c
onnectivities');
#19292=UNCERTAINTY_MEASURE_WITH_UNIT(LENGTH_MEASURE(0.001),#19362,
'DISTANCE_ACCURACY_VALUE',
'Maximum model space distance between geometric entities at asserted c
onnectivities');
#19293=UNCERTAINTY_MEASURE_WITH_UNIT(LENGTH_MEASURE(0.001),#19362,
'DISTANCE_ACCURACY_VALUE',
'Maximum model space distance between geometric entities at asserted c
onnectivities');
#19294=UNCERTAINTY_MEASURE_WITH_UNIT(LENGTH_MEASURE(0.001),#19362,
'DISTANCE_ACCURACY_VALUE',
'Maximum model space distance between geometric entities at asserted c
onnectivities');
#19295=UNCERTAINTY_MEASURE_WITH_UNIT(LENGTH_MEASURE(0.001),#19362,
'DISTANCE_ACCURACY_VALUE',
'Maximum model space distance between geometric entities at asserted c
onnectivities');
#19296=UNCERTAINTY_MEASURE_WITH_UNIT(LENGTH_MEASURE(0.001),#19362,
'DISTANCE_ACCURACY_VALUE',
'Maximum model space distance between geometric entities at asserted c
onnectivities');
#19297=UNCERTAINTY_MEASURE_WITH_UNIT(LENGTH_MEASURE(0.001),#19362,
'DISTANCE_ACCURACY_VALUE',
'Maximum model space distance between geometric entities at asserted c
onnectivities');
#19298=UNCERTAINTY_MEASURE_WITH_UNIT(LENGTH_MEASURE(0.001),#19362,
'DISTANCE_ACCURACY_VALUE',
'Maximum model space distance between geometric entities at asserted c
onnectivities');
#19299=UNCERTAINTY_MEASURE_WITH_UNIT(LENGTH_MEASURE(0.001),#19362,
'DISTANCE_ACCURACY_VALUE',
'Maximum model space distance between geometric entities at asserted c
onnectivities');
#19300=UNCERTAINTY_MEASURE_WITH_UNIT(LENGTH_MEASURE(0.001),#19362,
'DISTANCE_ACCURACY_VALUE',
'Maximum model space distance between geometric entities at asserted c
onnectivities');
#19301=UNCERTAINTY_MEASURE_WITH_UNIT(LENGTH_MEASURE(0.001),#19362,
'DISTANCE_ACCURACY_VALUE',
'Maximum model space distance between geometric entities at asserted c
onnectivities');
#19302=UNCERTAINTY_MEASURE_WITH_UNIT(LENGTH_MEASURE(0.001),#19362,
'DISTANCE_ACCURACY_VALUE',
'Maximum model space distance between geometric entities at asserted c
onnectivities');
#19303=UNCERTAINTY_MEASURE_WITH_UNIT(LENGTH_MEASURE(0.001),#19362,
'DISTANCE_ACCURACY_VALUE',
'Maximum model space distance between geometric entities at asserted c
onnectivities');
#19304=UNCERTAINTY_MEASURE_WITH_UNIT(LENGTH_MEASURE(0.001),#19362,
'DISTANCE_ACCURACY_VALUE',
'Maximum model space distance between geometric entities at asserted c
onnectivities');
#19305=UNCERTAINTY_MEASURE_WITH_UNIT(LENGTH_MEASURE(0.001),#19362,
'DISTANCE_ACCURACY_VALUE',
'Maximum model space distance between geometric entities at asserted c
onnectivities');
#19306=UNCERTAINTY_MEASURE_WITH_UNIT(LENGTH_MEASURE(0.001),#19362,
'DISTANCE_ACCURACY_VALUE',
'Maximum model space distance between geometric entities at asserted c
onnectivities');
#19307=UNCERTAINTY_MEASURE_WITH_UNIT(LENGTH_MEASURE(0.001),#19362,
'DISTANCE_ACCURACY_VALUE',
'Maximum model space distance between geometric entities at asserted c
onnectivities');
#19308=UNCERTAINTY_MEASURE_WITH_UNIT(LENGTH_MEASURE(0.001),#19362,
'DISTANCE_ACCURACY_VALUE',
'Maximum model space distance between geometric entities at asserted c
onnectivities');
#19309=UNCERTAINTY_MEASURE_WITH_UNIT(LENGTH_MEASURE(0.001),#19362,
'DISTANCE_ACCURACY_VALUE',
'Maximum model space distance between geometric entities at asserted c
onnectivities');
#19310=UNCERTAINTY_MEASURE_WITH_UNIT(LENGTH_MEASURE(0.001),#19362,
'DISTANCE_ACCURACY_VALUE',
'Maximum model space distance between geometric entities at asserted c
onnectivities');
#19311=UNCERTAINTY_MEASURE_WITH_UNIT(LENGTH_MEASURE(0.001),#19362,
'DISTANCE_ACCURACY_VALUE',
'Maximum model space distance between geometric entities at asserted c
onnectivities');
#19312=UNCERTAINTY_MEASURE_WITH_UNIT(LENGTH_MEASURE(0.001),#19362,
'DISTANCE_ACCURACY_VALUE',
'Maximum model space distance between geometric entities at asserted c
onnectivities');
#19313=UNCERTAINTY_MEASURE_WITH_UNIT(LENGTH_MEASURE(0.001),#19362,
'DISTANCE_ACCURACY_VALUE',
'Maximum model space distance between geometric entities at asserted c
onnectivities');
#19314=UNCERTAINTY_MEASURE_WITH_UNIT(LENGTH_MEASURE(0.001),#19362,
'DISTANCE_ACCURACY_VALUE',
'Maximum model space distance between geometric entities at asserted c
onnectivities');
#19315=UNCERTAINTY_MEASURE_WITH_UNIT(LENGTH_MEASURE(0.001),#19362,
'DISTANCE_ACCURACY_VALUE',
'Maximum model space distance between geometric entities at asserted c
onnectivities');
#19316=UNCERTAINTY_MEASURE_WITH_UNIT(LENGTH_MEASURE(0.001),#19362,
'DISTANCE_ACCURACY_VALUE',
'Maximum model space distance between geometric entities at asserted c
onnectivities');
#19317=UNCERTAINTY_MEASURE_WITH_UNIT(LENGTH_MEASURE(0.001),#19362,
'DISTANCE_ACCURACY_VALUE',
'Maximum model space distance between geometric entities at asserted c
onnectivities');
#19318=UNCERTAINTY_MEASURE_WITH_UNIT(LENGTH_MEASURE(0.001),#19362,
'DISTANCE_ACCURACY_VALUE',
'Maximum model space distance between geometric entities at asserted c
onnectivities');
#19319=UNCERTAINTY_MEASURE_WITH_UNIT(LENGTH_MEASURE(0.001),#19362,
'DISTANCE_ACCURACY_VALUE',
'Maximum model space distance between geometric entities at asserted c
onnectivities');
#19320=UNCERTAINTY_MEASURE_WITH_UNIT(LENGTH_MEASURE(0.001),#19362,
'DISTANCE_ACCURACY_VALUE',
'Maximum model space distance between geometric entities at asserted c
onnectivities');
#19321=UNCERTAINTY_MEASURE_WITH_UNIT(LENGTH_MEASURE(0.001),#19362,
'DISTANCE_ACCURACY_VALUE',
'Maximum model space distance between geometric entities at asserted c
onnectivities');
#19322=UNCERTAINTY_MEASURE_WITH_UNIT(LENGTH_MEASURE(0.001),#19362,
'DISTANCE_ACCURACY_VALUE',
'Maximum model space distance between geometric entities at asserted c
onnectivities');
#19323=UNCERTAINTY_MEASURE_WITH_UNIT(LENGTH_MEASURE(0.001),#19362,
'DISTANCE_ACCURACY_VALUE',
'Maximum model space distance between geometric entities at asserted c
onnectivities');
#19324=(
GEOMETRIC_REPRESENTATION_CONTEXT(3)
GLOBAL_UNCERTAINTY_ASSIGNED_CONTEXT((#19286))
GLOBAL_UNIT_ASSIGNED_CONTEXT((#19362,#19364,#19365))
REPRESENTATION_CONTEXT('','3D')
);
#19325=(
GEOMETRIC_REPRESENTATION_CONTEXT(3)
GLOBAL_UNCERTAINTY_ASSIGNED_CONTEXT((#19287))
GLOBAL_UNIT_ASSIGNED_CONTEXT((#19362,#19364,#19365))
REPRESENTATION_CONTEXT('','3D')
);
#19326=(
GEOMETRIC_REPRESENTATION_CONTEXT(3)
GLOBAL_UNCERTAINTY_ASSIGNED_CONTEXT((#19288))
GLOBAL_UNIT_ASSIGNED_CONTEXT((#19362,#19364,#19365))
REPRESENTATION_CONTEXT('','3D')
);
#19327=(
GEOMETRIC_REPRESENTATION_CONTEXT(3)
GLOBAL_UNCERTAINTY_ASSIGNED_CONTEXT((#19289))
GLOBAL_UNIT_ASSIGNED_CONTEXT((#19362,#19364,#19365))
REPRESENTATION_CONTEXT('','3D')
);
#19328=(
GEOMETRIC_REPRESENTATION_CONTEXT(3)
GLOBAL_UNCERTAINTY_ASSIGNED_CONTEXT((#19290))
GLOBAL_UNIT_ASSIGNED_CONTEXT((#19362,#19364,#19365))
REPRESENTATION_CONTEXT('','3D')
);
#19329=(
GEOMETRIC_REPRESENTATION_CONTEXT(3)
GLOBAL_UNCERTAINTY_ASSIGNED_CONTEXT((#19291))
GLOBAL_UNIT_ASSIGNED_CONTEXT((#19362,#19364,#19365))
REPRESENTATION_CONTEXT('','3D')
);
#19330=(
GEOMETRIC_REPRESENTATION_CONTEXT(3)
GLOBAL_UNCERTAINTY_ASSIGNED_CONTEXT((#19292))
GLOBAL_UNIT_ASSIGNED_CONTEXT((#19362,#19364,#19365))
REPRESENTATION_CONTEXT('','3D')
);
#19331=(
GEOMETRIC_REPRESENTATION_CONTEXT(3)
GLOBAL_UNCERTAINTY_ASSIGNED_CONTEXT((#19293))
GLOBAL_UNIT_ASSIGNED_CONTEXT((#19362,#19364,#19365))
REPRESENTATION_CONTEXT('','3D')
);
#19332=(
GEOMETRIC_REPRESENTATION_CONTEXT(3)
GLOBAL_UNCERTAINTY_ASSIGNED_CONTEXT((#19294))
GLOBAL_UNIT_ASSIGNED_CONTEXT((#19362,#19364,#19365))
REPRESENTATION_CONTEXT('','3D')
);
#19333=(
GEOMETRIC_REPRESENTATION_CONTEXT(3)
GLOBAL_UNCERTAINTY_ASSIGNED_CONTEXT((#19295))
GLOBAL_UNIT_ASSIGNED_CONTEXT((#19362,#19364,#19365))
REPRESENTATION_CONTEXT('','3D')
);
#19334=(
GEOMETRIC_REPRESENTATION_CONTEXT(3)
GLOBAL_UNCERTAINTY_ASSIGNED_CONTEXT((#19296))
GLOBAL_UNIT_ASSIGNED_CONTEXT((#19362,#19364,#19365))
REPRESENTATION_CONTEXT('','3D')
);
#19335=(
GEOMETRIC_REPRESENTATION_CONTEXT(3)
GLOBAL_UNCERTAINTY_ASSIGNED_CONTEXT((#19297))
GLOBAL_UNIT_ASSIGNED_CONTEXT((#19362,#19364,#19365))
REPRESENTATION_CONTEXT('','3D')
);
#19336=(
GEOMETRIC_REPRESENTATION_CONTEXT(3)
GLOBAL_UNCERTAINTY_ASSIGNED_CONTEXT((#19298))
GLOBAL_UNIT_ASSIGNED_CONTEXT((#19362,#19364,#19365))
REPRESENTATION_CONTEXT('','3D')
);
#19337=(
GEOMETRIC_REPRESENTATION_CONTEXT(3)
GLOBAL_UNCERTAINTY_ASSIGNED_CONTEXT((#19299))
GLOBAL_UNIT_ASSIGNED_CONTEXT((#19362,#19364,#19365))
REPRESENTATION_CONTEXT('','3D')
);
#19338=(
GEOMETRIC_REPRESENTATION_CONTEXT(3)
GLOBAL_UNCERTAINTY_ASSIGNED_CONTEXT((#19300))
GLOBAL_UNIT_ASSIGNED_CONTEXT((#19362,#19364,#19365))
REPRESENTATION_CONTEXT('','3D')
);
#19339=(
GEOMETRIC_REPRESENTATION_CONTEXT(3)
GLOBAL_UNCERTAINTY_ASSIGNED_CONTEXT((#19301))
GLOBAL_UNIT_ASSIGNED_CONTEXT((#19362,#19364,#19365))
REPRESENTATION_CONTEXT('','3D')
);
#19340=(
GEOMETRIC_REPRESENTATION_CONTEXT(3)
GLOBAL_UNCERTAINTY_ASSIGNED_CONTEXT((#19302))
GLOBAL_UNIT_ASSIGNED_CONTEXT((#19362,#19364,#19365))
REPRESENTATION_CONTEXT('','3D')
);
#19341=(
GEOMETRIC_REPRESENTATION_CONTEXT(3)
GLOBAL_UNCERTAINTY_ASSIGNED_CONTEXT((#19303))
GLOBAL_UNIT_ASSIGNED_CONTEXT((#19362,#19364,#19365))
REPRESENTATION_CONTEXT('','3D')
);
#19342=(
GEOMETRIC_REPRESENTATION_CONTEXT(3)
GLOBAL_UNCERTAINTY_ASSIGNED_CONTEXT((#19304))
GLOBAL_UNIT_ASSIGNED_CONTEXT((#19362,#19364,#19365))
REPRESENTATION_CONTEXT('','3D')
);
#19343=(
GEOMETRIC_REPRESENTATION_CONTEXT(3)
GLOBAL_UNCERTAINTY_ASSIGNED_CONTEXT((#19305))
GLOBAL_UNIT_ASSIGNED_CONTEXT((#19362,#19364,#19365))
REPRESENTATION_CONTEXT('','3D')
);
#19344=(
GEOMETRIC_REPRESENTATION_CONTEXT(3)
GLOBAL_UNCERTAINTY_ASSIGNED_CONTEXT((#19306))
GLOBAL_UNIT_ASSIGNED_CONTEXT((#19362,#19364,#19365))
REPRESENTATION_CONTEXT('','3D')
);
#19345=(
GEOMETRIC_REPRESENTATION_CONTEXT(3)
GLOBAL_UNCERTAINTY_ASSIGNED_CONTEXT((#19307))
GLOBAL_UNIT_ASSIGNED_CONTEXT((#19362,#19364,#19365))
REPRESENTATION_CONTEXT('','3D')
);
#19346=(
GEOMETRIC_REPRESENTATION_CONTEXT(3)
GLOBAL_UNCERTAINTY_ASSIGNED_CONTEXT((#19308))
GLOBAL_UNIT_ASSIGNED_CONTEXT((#19362,#19364,#19365))
REPRESENTATION_CONTEXT('','3D')
);
#19347=(
GEOMETRIC_REPRESENTATION_CONTEXT(3)
GLOBAL_UNCERTAINTY_ASSIGNED_CONTEXT((#19309))
GLOBAL_UNIT_ASSIGNED_CONTEXT((#19362,#19364,#19365))
REPRESENTATION_CONTEXT('','3D')
);
#19348=(
GEOMETRIC_REPRESENTATION_CONTEXT(3)
GLOBAL_UNCERTAINTY_ASSIGNED_CONTEXT((#19310))
GLOBAL_UNIT_ASSIGNED_CONTEXT((#19362,#19364,#19365))
REPRESENTATION_CONTEXT('','3D')
);
#19349=(
GEOMETRIC_REPRESENTATION_CONTEXT(3)
GLOBAL_UNCERTAINTY_ASSIGNED_CONTEXT((#19311))
GLOBAL_UNIT_ASSIGNED_CONTEXT((#19362,#19364,#19365))
REPRESENTATION_CONTEXT('','3D')
);
#19350=(
GEOMETRIC_REPRESENTATION_CONTEXT(3)
GLOBAL_UNCERTAINTY_ASSIGNED_CONTEXT((#19312))
GLOBAL_UNIT_ASSIGNED_CONTEXT((#19362,#19364,#19365))
REPRESENTATION_CONTEXT('','3D')
);
#19351=(
GEOMETRIC_REPRESENTATION_CONTEXT(3)
GLOBAL_UNCERTAINTY_ASSIGNED_CONTEXT((#19313))
GLOBAL_UNIT_ASSIGNED_CONTEXT((#19362,#19364,#19365))
REPRESENTATION_CONTEXT('','3D')
);
#19352=(
GEOMETRIC_REPRESENTATION_CONTEXT(3)
GLOBAL_UNCERTAINTY_ASSIGNED_CONTEXT((#19314))
GLOBAL_UNIT_ASSIGNED_CONTEXT((#19362,#19364,#19365))
REPRESENTATION_CONTEXT('','3D')
);
#19353=(
GEOMETRIC_REPRESENTATION_CONTEXT(3)
GLOBAL_UNCERTAINTY_ASSIGNED_CONTEXT((#19315))
GLOBAL_UNIT_ASSIGNED_CONTEXT((#19362,#19364,#19365))
REPRESENTATION_CONTEXT('','3D')
);
#19354=(
GEOMETRIC_REPRESENTATION_CONTEXT(3)
GLOBAL_UNCERTAINTY_ASSIGNED_CONTEXT((#19316))
GLOBAL_UNIT_ASSIGNED_CONTEXT((#19362,#19364,#19365))
REPRESENTATION_CONTEXT('','3D')
);
#19355=(
GEOMETRIC_REPRESENTATION_CONTEXT(3)
GLOBAL_UNCERTAINTY_ASSIGNED_CONTEXT((#19317))
GLOBAL_UNIT_ASSIGNED_CONTEXT((#19362,#19364,#19365))
REPRESENTATION_CONTEXT('','3D')
);
#19356=(
GEOMETRIC_REPRESENTATION_CONTEXT(3)
GLOBAL_UNCERTAINTY_ASSIGNED_CONTEXT((#19318))
GLOBAL_UNIT_ASSIGNED_CONTEXT((#19362,#19364,#19365))
REPRESENTATION_CONTEXT('','3D')
);
#19357=(
GEOMETRIC_REPRESENTATION_CONTEXT(3)
GLOBAL_UNCERTAINTY_ASSIGNED_CONTEXT((#19319))
GLOBAL_UNIT_ASSIGNED_CONTEXT((#19362,#19364,#19365))
REPRESENTATION_CONTEXT('','3D')
);
#19358=(
GEOMETRIC_REPRESENTATION_CONTEXT(3)
GLOBAL_UNCERTAINTY_ASSIGNED_CONTEXT((#19320))
GLOBAL_UNIT_ASSIGNED_CONTEXT((#19362,#19364,#19365))
REPRESENTATION_CONTEXT('','3D')
);
#19359=(
GEOMETRIC_REPRESENTATION_CONTEXT(3)
GLOBAL_UNCERTAINTY_ASSIGNED_CONTEXT((#19321))
GLOBAL_UNIT_ASSIGNED_CONTEXT((#19362,#19364,#19365))
REPRESENTATION_CONTEXT('','3D')
);
#19360=(
GEOMETRIC_REPRESENTATION_CONTEXT(3)
GLOBAL_UNCERTAINTY_ASSIGNED_CONTEXT((#19322))
GLOBAL_UNIT_ASSIGNED_CONTEXT((#19362,#19364,#19365))
REPRESENTATION_CONTEXT('','3D')
);
#19361=(
GEOMETRIC_REPRESENTATION_CONTEXT(3)
GLOBAL_UNCERTAINTY_ASSIGNED_CONTEXT((#19323))
GLOBAL_UNIT_ASSIGNED_CONTEXT((#19362,#19364,#19365))
REPRESENTATION_CONTEXT('','3D')
);
#19362=(
LENGTH_UNIT()
NAMED_UNIT(*)
SI_UNIT(.CENTI.,.METRE.)
);
#19363=(
LENGTH_UNIT()
NAMED_UNIT(*)
SI_UNIT($,.METRE.)
);
#19364=(
NAMED_UNIT(*)
PLANE_ANGLE_UNIT()
SI_UNIT($,.RADIAN.)
);
#19365=(
NAMED_UNIT(*)
SI_UNIT($,.STERADIAN.)
SOLID_ANGLE_UNIT()
);
#19366=SHAPE_DEFINITION_REPRESENTATION(#19403,#19488);
#19367=SHAPE_DEFINITION_REPRESENTATION(#19404,#19489);
#19368=SHAPE_DEFINITION_REPRESENTATION(#19405,#19490);
#19369=SHAPE_DEFINITION_REPRESENTATION(#19406,#19491);
#19370=SHAPE_DEFINITION_REPRESENTATION(#19407,#19492);
#19371=SHAPE_DEFINITION_REPRESENTATION(#19408,#19493);
#19372=SHAPE_DEFINITION_REPRESENTATION(#19409,#19494);
#19373=SHAPE_DEFINITION_REPRESENTATION(#19410,#19495);
#19374=SHAPE_DEFINITION_REPRESENTATION(#19411,#19496);
#19375=SHAPE_DEFINITION_REPRESENTATION(#19412,#19497);
#19376=SHAPE_DEFINITION_REPRESENTATION(#19413,#19498);
#19377=SHAPE_DEFINITION_REPRESENTATION(#19414,#19499);
#19378=SHAPE_DEFINITION_REPRESENTATION(#19415,#19500);
#19379=SHAPE_DEFINITION_REPRESENTATION(#19416,#19501);
#19380=SHAPE_DEFINITION_REPRESENTATION(#19417,#19502);
#19381=SHAPE_DEFINITION_REPRESENTATION(#19418,#19503);
#19382=SHAPE_DEFINITION_REPRESENTATION(#19419,#19504);
#19383=SHAPE_DEFINITION_REPRESENTATION(#19420,#19505);
#19384=SHAPE_DEFINITION_REPRESENTATION(#19423,#19506);
#19385=SHAPE_DEFINITION_REPRESENTATION(#19424,#19507);
#19386=SHAPE_DEFINITION_REPRESENTATION(#19425,#19508);
#19387=SHAPE_DEFINITION_REPRESENTATION(#19451,#19509);
#19388=SHAPE_DEFINITION_REPRESENTATION(#19452,#19510);
#19389=SHAPE_DEFINITION_REPRESENTATION(#19453,#19511);
#19390=SHAPE_DEFINITION_REPRESENTATION(#19454,#19512);
#19391=SHAPE_DEFINITION_REPRESENTATION(#19455,#19513);
#19392=SHAPE_DEFINITION_REPRESENTATION(#19456,#19514);
#19393=SHAPE_DEFINITION_REPRESENTATION(#19457,#19515);
#19394=SHAPE_DEFINITION_REPRESENTATION(#19458,#19516);
#19395=SHAPE_DEFINITION_REPRESENTATION(#19459,#19517);
#19396=SHAPE_DEFINITION_REPRESENTATION(#19460,#19518);
#19397=SHAPE_DEFINITION_REPRESENTATION(#19461,#19519);
#19398=SHAPE_DEFINITION_REPRESENTATION(#19462,#19520);
#19399=SHAPE_DEFINITION_REPRESENTATION(#19463,#19521);
#19400=SHAPE_DEFINITION_REPRESENTATION(#19467,#19522);
#19401=SHAPE_DEFINITION_REPRESENTATION(#19468,#19523);
#19402=SHAPE_DEFINITION_REPRESENTATION(#19469,#19524);
#19403=PRODUCT_DEFINITION_SHAPE('',$,#19526);
#19404=PRODUCT_DEFINITION_SHAPE('',$,#19527);
#19405=PRODUCT_DEFINITION_SHAPE('',$,#19528);
#19406=PRODUCT_DEFINITION_SHAPE('',$,#19529);
#19407=PRODUCT_DEFINITION_SHAPE('',$,#19530);
#19408=PRODUCT_DEFINITION_SHAPE('',$,#19531);
#19409=PRODUCT_DEFINITION_SHAPE('',$,#19532);
#19410=PRODUCT_DEFINITION_SHAPE('',$,#19533);
#19411=PRODUCT_DEFINITION_SHAPE('',$,#19534);
#19412=PRODUCT_DEFINITION_SHAPE('',$,#19535);
#19413=PRODUCT_DEFINITION_SHAPE('',$,#19536);
#19414=PRODUCT_DEFINITION_SHAPE('',$,#19537);
#19415=PRODUCT_DEFINITION_SHAPE('',$,#19538);
#19416=PRODUCT_DEFINITION_SHAPE('',$,#19539);
#19417=PRODUCT_DEFINITION_SHAPE('',$,#19540);
#19418=PRODUCT_DEFINITION_SHAPE('',$,#19541);
#19419=PRODUCT_DEFINITION_SHAPE('',$,#19542);
#19420=PRODUCT_DEFINITION_SHAPE('',$,#19543);
#19421=PRODUCT_DEFINITION_SHAPE($,$,#179);
#19422=PRODUCT_DEFINITION_SHAPE($,$,#180);
#19423=PRODUCT_DEFINITION_SHAPE('',$,#19544);
#19424=PRODUCT_DEFINITION_SHAPE('',$,#19545);
#19425=PRODUCT_DEFINITION_SHAPE('',$,#19546);
#19426=PRODUCT_DEFINITION_SHAPE($,$,#181);
#19427=PRODUCT_DEFINITION_SHAPE($,$,#182);
#19428=PRODUCT_DEFINITION_SHAPE($,$,#183);
#19429=PRODUCT_DEFINITION_SHAPE($,$,#184);
#19430=PRODUCT_DEFINITION_SHAPE($,$,#185);
#19431=PRODUCT_DEFINITION_SHAPE($,$,#186);
#19432=PRODUCT_DEFINITION_SHAPE($,$,#187);
#19433=PRODUCT_DEFINITION_SHAPE($,$,#188);
#19434=PRODUCT_DEFINITION_SHAPE($,$,#189);
#19435=PRODUCT_DEFINITION_SHAPE($,$,#190);
#19436=PRODUCT_DEFINITION_SHAPE($,$,#191);
#19437=PRODUCT_DEFINITION_SHAPE($,$,#192);
#19438=PRODUCT_DEFINITION_SHAPE($,$,#193);
#19439=PRODUCT_DEFINITION_SHAPE($,$,#194);
#19440=PRODUCT_DEFINITION_SHAPE($,$,#195);
#19441=PRODUCT_DEFINITION_SHAPE($,$,#196);
#19442=PRODUCT_DEFINITION_SHAPE($,$,#197);
#19443=PRODUCT_DEFINITION_SHAPE($,$,#198);
#19444=PRODUCT_DEFINITION_SHAPE($,$,#199);
#19445=PRODUCT_DEFINITION_SHAPE($,$,#200);
#19446=PRODUCT_DEFINITION_SHAPE($,$,#201);
#19447=PRODUCT_DEFINITION_SHAPE($,$,#202);
#19448=PRODUCT_DEFINITION_SHAPE($,$,#203);
#19449=PRODUCT_DEFINITION_SHAPE($,$,#204);
#19450=PRODUCT_DEFINITION_SHAPE($,$,#205);
#19451=PRODUCT_DEFINITION_SHAPE('',$,#19547);
#19452=PRODUCT_DEFINITION_SHAPE('',$,#19548);
#19453=PRODUCT_DEFINITION_SHAPE('',$,#19549);
#19454=PRODUCT_DEFINITION_SHAPE('',$,#19550);
#19455=PRODUCT_DEFINITION_SHAPE('',$,#19551);
#19456=PRODUCT_DEFINITION_SHAPE('',$,#19552);
#19457=PRODUCT_DEFINITION_SHAPE('',$,#19553);
#19458=PRODUCT_DEFINITION_SHAPE('',$,#19554);
#19459=PRODUCT_DEFINITION_SHAPE('',$,#19555);
#19460=PRODUCT_DEFINITION_SHAPE('',$,#19556);
#19461=PRODUCT_DEFINITION_SHAPE('',$,#19557);
#19462=PRODUCT_DEFINITION_SHAPE('',$,#19558);
#19463=PRODUCT_DEFINITION_SHAPE('',$,#19559);
#19464=PRODUCT_DEFINITION_SHAPE($,$,#206);
#19465=PRODUCT_DEFINITION_SHAPE($,$,#207);
#19466=PRODUCT_DEFINITION_SHAPE($,$,#208);
#19467=PRODUCT_DEFINITION_SHAPE('',$,#19560);
#19468=PRODUCT_DEFINITION_SHAPE('',$,#19561);
#19469=PRODUCT_DEFINITION_SHAPE('',$,#19562);
#19470=PRODUCT_DEFINITION_SHAPE($,$,#209);
#19471=PRODUCT_DEFINITION_SHAPE($,$,#210);
#19472=PRODUCT_DEFINITION_SHAPE($,$,#211);
#19473=PRODUCT_DEFINITION_SHAPE($,$,#212);
#19474=PRODUCT_DEFINITION_SHAPE($,$,#213);
#19475=PRODUCT_DEFINITION_SHAPE($,$,#214);
#19476=PRODUCT_DEFINITION_SHAPE($,$,#215);
#19477=PRODUCT_DEFINITION_SHAPE($,$,#216);
#19478=PRODUCT_DEFINITION_SHAPE($,$,#217);
#19479=PRODUCT_DEFINITION_SHAPE($,$,#218);
#19480=PRODUCT_DEFINITION_SHAPE($,$,#219);
#19481=PRODUCT_DEFINITION_SHAPE($,$,#220);
#19482=PRODUCT_DEFINITION_SHAPE($,$,#221);
#19483=PRODUCT_DEFINITION_SHAPE($,$,#222);
#19484=PRODUCT_DEFINITION_SHAPE($,$,#223);
#19485=PRODUCT_DEFINITION_SHAPE($,$,#224);
#19486=PRODUCT_DEFINITION_SHAPE($,$,#225);
#19487=PRODUCT_DEFINITION_SHAPE($,$,#226);
#19488=SHAPE_REPRESENTATION('',(#11373,#12338,#12339),#19324);
#19489=SHAPE_REPRESENTATION('',(#11374,#11717,#11718,#11719,#11720,#11721,
#11722,#11723,#11724,#11725,#11726,#11727,#11728,#11729,#11730,#11731,#11732,
#11733,#11734,#11735,#11736,#11737,#11738,#11739,#11740,#11741),#19325);
#19490=SHAPE_REPRESENTATION('',(#11375),#19326);
#19491=SHAPE_REPRESENTATION('',(#11400),#19327);
#19492=SHAPE_REPRESENTATION('',(#11407),#19328);
#19493=SHAPE_REPRESENTATION('',(#11414),#19329);
#19494=SHAPE_REPRESENTATION('',(#11423),#19330);
#19495=SHAPE_REPRESENTATION('',(#11432),#19331);
#19496=SHAPE_REPRESENTATION('',(#11441),#19332);
#19497=SHAPE_REPRESENTATION('',(#11450),#19333);
#19498=SHAPE_REPRESENTATION('',(#11480),#19334);
#19499=SHAPE_REPRESENTATION('',(#11510),#19335);
#19500=SHAPE_REPRESENTATION('',(#11527),#19336);
#19501=SHAPE_REPRESENTATION('',(#11544),#19337);
#19502=SHAPE_REPRESENTATION('',(#11561),#19338);
#19503=SHAPE_REPRESENTATION('',(#11578,#11658,#11659),#19339);
#19504=SHAPE_REPRESENTATION('',(#11579),#19340);
#19505=SHAPE_REPRESENTATION('',(#11630),#19341);
#19506=SHAPE_REPRESENTATION('',(#11660),#19342);
#19507=SHAPE_REPRESENTATION('',(#11669),#19343);
#19508=SHAPE_REPRESENTATION('',(#11693),#19344);
#19509=SHAPE_REPRESENTATION('',(#11742,#12322,#12323,#12324,#12325,#12326,
#12327,#12328,#12329,#12330,#12331,#12332,#12333,#12334,#12335,#12336,#12337),
#19345);
#19510=SHAPE_REPRESENTATION('',(#11743),#19346);
#19511=SHAPE_REPRESENTATION('',(#11760),#19347);
#19512=SHAPE_REPRESENTATION('',(#11766),#19348);
#19513=SHAPE_REPRESENTATION('',(#11781),#19349);
#19514=SHAPE_REPRESENTATION('',(#11807),#19350);
#19515=SHAPE_REPRESENTATION('',(#11822),#19351);
#19516=SHAPE_REPRESENTATION('',(#11837),#19352);
#19517=SHAPE_REPRESENTATION('',(#11846),#19353);
#19518=SHAPE_REPRESENTATION('',(#11863,#12253,#12254,#12255),#19354);
#19519=SHAPE_REPRESENTATION('',(#11864),#19355);
#19520=SHAPE_REPRESENTATION('',(#11982),#19356);
#19521=SHAPE_REPRESENTATION('',(#12100),#19357);
#19522=SHAPE_REPRESENTATION('',(#12256),#19358);
#19523=SHAPE_REPRESENTATION('',(#12279),#19359);
#19524=SHAPE_REPRESENTATION('',(#12296),#19360);
#19525=PRODUCT_DEFINITION_CONTEXT('part definition',#19638,'design');
#19526=PRODUCT_DEFINITION('PAT-062',
'PAT-062',#19563,#19525);
#19527=PRODUCT_DEFINITION('Motor and bearing base',
'Motor and bearing base',#19564,#19525);
#19528=PRODUCT_DEFINITION('Base','Base',#19565,#19525);
#19529=PRODUCT_DEFINITION('Bonded pad','Bonded pad',#19566,#19525);
#19530=PRODUCT_DEFINITION('Bonded pad (1)','Bonded pad (1)',#19567,#19525);
#19531=PRODUCT_DEFINITION('Mounting reducer','Mounting reducer',#19568,
#19525);
#19532=PRODUCT_DEFINITION('Mounting reducer (1)','Mounting reducer (1)',#19569,
#19525);
#19533=PRODUCT_DEFINITION('Mounting reducer (2)','Mounting reducer (2)',#19570,
#19525);
#19534=PRODUCT_DEFINITION('Mounting reducer (3)','Mounting reducer (3)',#19571,
#19525);
#19535=PRODUCT_DEFINITION('Motor bracket','Motor bracket',#19572,#19525);
#19536=PRODUCT_DEFINITION('Motor envelope','Motor envelope',#19573,#19525);
#19537=PRODUCT_DEFINITION('M3x10 motor screw','M3x10 motor screw',#19574,
#19525);
#19538=PRODUCT_DEFINITION('M3x10 motor screw (1)','M3x10 motor screw (1)',
#19575,#19525);
#19539=PRODUCT_DEFINITION('M3x10 motor screw (2)','M3x10 motor screw (2)',
#19576,#19525);
#19540=PRODUCT_DEFINITION('M3x10 motor screw (3)','M3x10 motor screw (3)',
#19577,#19525);
#19541=PRODUCT_DEFINITION('Pillow Block Bearing - 12 mm Bore',
'Pillow Block Bearing - 12 mm Bore',#19578,#19525);
#19542=PRODUCT_DEFINITION('Housing','Housing',#19579,#19525);
#19543=PRODUCT_DEFINITION('Insert bearing','Insert bearing',#19580,#19525);
#19544=PRODUCT_DEFINITION('Flat Washer - M8','Flat Washer - M8',#19581,
#19525);
#19545=PRODUCT_DEFINITION('M8x25 Bolt','M8x25 Bolt',#19582,#19525);
#19546=PRODUCT_DEFINITION('M5x14 Cap Screw','M5x14 Cap Screw',#19583,#19525);
#19547=PRODUCT_DEFINITION('Coupled rotor','Coupled rotor',#19584,#19525);
#19548=PRODUCT_DEFINITION('Driven shaft','Driven shaft',#19585,#19525);
#19549=PRODUCT_DEFINITION('Motor rotor shaft','Motor rotor shaft',#19586,
#19525);
#19550=PRODUCT_DEFINITION('Motor shaft adapter','Motor shaft adapter',#19587,
#19525);
#19551=PRODUCT_DEFINITION('Flywheel','Flywheel',#19588,#19525);
#19552=PRODUCT_DEFINITION('Shaft collar','Shaft collar',#19589,#19525);
#19553=PRODUCT_DEFINITION('Shaft collar (1)','Shaft collar (1)',#19590,#19525);
#19554=PRODUCT_DEFINITION('Shaft end keeper','Shaft end keeper',#19591,
#19525);
#19555=PRODUCT_DEFINITION('Socket Set Screw - M4x6',
'Socket Set Screw - M4x6',#19592,#19525);
#19556=PRODUCT_DEFINITION('Flexible Jaw Coupling - 12 mm Bores',
'Flexible Jaw Coupling - 12 mm Bores',#19593,#19525);
#19557=PRODUCT_DEFINITION('Hub A','Hub A',#19594,#19525);
#19558=PRODUCT_DEFINITION('Hub B','Hub B',#19595,#19525);
#19559=PRODUCT_DEFINITION('Spider','Spider',#19596,#19525);
#19560=PRODUCT_DEFINITION('Parallel Key - 4x4x20',
'Parallel Key - 4x4x20',#19597,#19525);
#19561=PRODUCT_DEFINITION('Socket Set Screw - M5x8',
'Socket Set Screw - M5x8',#19598,#19525);
#19562=PRODUCT_DEFINITION('Cap Screw - M4x16','Cap Screw - M4x16',#19599,
#19525);
#19563=PRODUCT_DEFINITION_FORMATION('',$,#19640);
#19564=PRODUCT_DEFINITION_FORMATION('',$,#19641);
#19565=PRODUCT_DEFINITION_FORMATION('',$,#19642);
#19566=PRODUCT_DEFINITION_FORMATION('',$,#19643);
#19567=PRODUCT_DEFINITION_FORMATION('',$,#19644);
#19568=PRODUCT_DEFINITION_FORMATION('',$,#19645);
#19569=PRODUCT_DEFINITION_FORMATION('',$,#19646);
#19570=PRODUCT_DEFINITION_FORMATION('',$,#19647);
#19571=PRODUCT_DEFINITION_FORMATION('',$,#19648);
#19572=PRODUCT_DEFINITION_FORMATION('',$,#19649);
#19573=PRODUCT_DEFINITION_FORMATION('',$,#19650);
#19574=PRODUCT_DEFINITION_FORMATION('',$,#19651);
#19575=PRODUCT_DEFINITION_FORMATION('',$,#19652);
#19576=PRODUCT_DEFINITION_FORMATION('',$,#19653);
#19577=PRODUCT_DEFINITION_FORMATION('',$,#19654);
#19578=PRODUCT_DEFINITION_FORMATION('',$,#19655);
#19579=PRODUCT_DEFINITION_FORMATION('',$,#19656);
#19580=PRODUCT_DEFINITION_FORMATION('',$,#19657);
#19581=PRODUCT_DEFINITION_FORMATION('',$,#19658);
#19582=PRODUCT_DEFINITION_FORMATION('',$,#19659);
#19583=PRODUCT_DEFINITION_FORMATION('',$,#19660);
#19584=PRODUCT_DEFINITION_FORMATION('',$,#19661);
#19585=PRODUCT_DEFINITION_FORMATION('',$,#19662);
#19586=PRODUCT_DEFINITION_FORMATION('',$,#19663);
#19587=PRODUCT_DEFINITION_FORMATION('',$,#19664);
#19588=PRODUCT_DEFINITION_FORMATION('',$,#19665);
#19589=PRODUCT_DEFINITION_FORMATION('',$,#19666);
#19590=PRODUCT_DEFINITION_FORMATION('',$,#19667);
#19591=PRODUCT_DEFINITION_FORMATION('',$,#19668);
#19592=PRODUCT_DEFINITION_FORMATION('',$,#19669);
#19593=PRODUCT_DEFINITION_FORMATION('',$,#19670);
#19594=PRODUCT_DEFINITION_FORMATION('',$,#19671);
#19595=PRODUCT_DEFINITION_FORMATION('',$,#19672);
#19596=PRODUCT_DEFINITION_FORMATION('',$,#19673);
#19597=PRODUCT_DEFINITION_FORMATION('',$,#19674);
#19598=PRODUCT_DEFINITION_FORMATION('',$,#19675);
#19599=PRODUCT_DEFINITION_FORMATION('',$,#19676);
#19600=PRODUCT_RELATED_PRODUCT_CATEGORY('PAT-062','PAT-062',(#19640));
#19601=PRODUCT_RELATED_PRODUCT_CATEGORY('Motor and bearing base',
'Motor and bearing base',(#19641));
#19602=PRODUCT_RELATED_PRODUCT_CATEGORY('Base','Base',(#19642));
#19603=PRODUCT_RELATED_PRODUCT_CATEGORY('Bonded pad','Bonded pad',(#19643));
#19604=PRODUCT_RELATED_PRODUCT_CATEGORY('Bonded pad (1)',
'Bonded pad (1)',(#19644));
#19605=PRODUCT_RELATED_PRODUCT_CATEGORY('Mounting reducer',
'Mounting reducer',(#19645));
#19606=PRODUCT_RELATED_PRODUCT_CATEGORY('Mounting reducer (1)',
'Mounting reducer (1)',(#19646));
#19607=PRODUCT_RELATED_PRODUCT_CATEGORY('Mounting reducer (2)',
'Mounting reducer (2)',(#19647));
#19608=PRODUCT_RELATED_PRODUCT_CATEGORY('Mounting reducer (3)',
'Mounting reducer (3)',(#19648));
#19609=PRODUCT_RELATED_PRODUCT_CATEGORY('Motor bracket','Motor bracket',
(#19649));
#19610=PRODUCT_RELATED_PRODUCT_CATEGORY('Motor envelope',
'Motor envelope',(#19650));
#19611=PRODUCT_RELATED_PRODUCT_CATEGORY('M3x10 motor screw',
'M3x10 motor screw',(#19651));
#19612=PRODUCT_RELATED_PRODUCT_CATEGORY('M3x10 motor screw (1)',
'M3x10 motor screw (1)',(#19652));
#19613=PRODUCT_RELATED_PRODUCT_CATEGORY('M3x10 motor screw (2)',
'M3x10 motor screw (2)',(#19653));
#19614=PRODUCT_RELATED_PRODUCT_CATEGORY('M3x10 motor screw (3)',
'M3x10 motor screw (3)',(#19654));
#19615=PRODUCT_RELATED_PRODUCT_CATEGORY(
'Pillow Block Bearing - 12 mm Bore','Pillow Block Bearing - 12 mm Bore',
(#19655));
#19616=PRODUCT_RELATED_PRODUCT_CATEGORY('Housing','Housing',(#19656));
#19617=PRODUCT_RELATED_PRODUCT_CATEGORY('Insert bearing',
'Insert bearing',(#19657));
#19618=PRODUCT_RELATED_PRODUCT_CATEGORY('Flat Washer - M8',
'Flat Washer - M8',(#19658));
#19619=PRODUCT_RELATED_PRODUCT_CATEGORY('M8x25 Bolt','M8x25 Bolt',(#19659));
#19620=PRODUCT_RELATED_PRODUCT_CATEGORY('M5x14 Cap Screw',
'M5x14 Cap Screw',(#19660));
#19621=PRODUCT_RELATED_PRODUCT_CATEGORY('Coupled rotor','Coupled rotor',
(#19661));
#19622=PRODUCT_RELATED_PRODUCT_CATEGORY('Driven shaft','Driven shaft',(#19662));
#19623=PRODUCT_RELATED_PRODUCT_CATEGORY('Motor rotor shaft',
'Motor rotor shaft',(#19663));
#19624=PRODUCT_RELATED_PRODUCT_CATEGORY('Motor shaft adapter',
'Motor shaft adapter',(#19664));
#19625=PRODUCT_RELATED_PRODUCT_CATEGORY('Flywheel','Flywheel',(#19665));
#19626=PRODUCT_RELATED_PRODUCT_CATEGORY('Shaft collar','Shaft collar',(#19666));
#19627=PRODUCT_RELATED_PRODUCT_CATEGORY('Shaft collar (1)',
'Shaft collar (1)',(#19667));
#19628=PRODUCT_RELATED_PRODUCT_CATEGORY('Shaft end keeper',
'Shaft end keeper',(#19668));
#19629=PRODUCT_RELATED_PRODUCT_CATEGORY('Socket Set Screw - M4x6',
'Socket Set Screw - M4x6',(#19669));
#19630=PRODUCT_RELATED_PRODUCT_CATEGORY(
'Flexible Jaw Coupling - 12 mm Bores',
'Flexible Jaw Coupling - 12 mm Bores',(#19670));
#19631=PRODUCT_RELATED_PRODUCT_CATEGORY('Hub A','Hub A',(#19671));
#19632=PRODUCT_RELATED_PRODUCT_CATEGORY('Hub B','Hub B',(#19672));
#19633=PRODUCT_RELATED_PRODUCT_CATEGORY('Spider','Spider',(#19673));
#19634=PRODUCT_RELATED_PRODUCT_CATEGORY('Parallel Key - 4x4x20',
'Parallel Key - 4x4x20',(#19674));
#19635=PRODUCT_RELATED_PRODUCT_CATEGORY('Socket Set Screw - M5x8',
'Socket Set Screw - M5x8',(#19675));
#19636=PRODUCT_RELATED_PRODUCT_CATEGORY('Cap Screw - M4x16',
'Cap Screw - M4x16',(#19676));
#19637=APPLICATION_PROTOCOL_DEFINITION('international standard',
'automotive_design',2009,#19638);
#19638=APPLICATION_CONTEXT(
'Core Data for Automotive Mechanical Design Process');
#19639=PRODUCT_CONTEXT('part definition',#19638,'mechanical');
#19640=PRODUCT('PAT-062','PAT-062',
'PAT-062',(#19639));
#19641=PRODUCT('Motor and bearing base','Motor and bearing base',
'Motor and bearing base',(#19639));
#19642=PRODUCT('Base','Base','Base',(#19639));
#19643=PRODUCT('Bonded pad','Bonded pad','Bonded pad',(#19639));
#19644=PRODUCT('Bonded pad (1)','Bonded pad (1)','Bonded pad (1)',(#19639));
#19645=PRODUCT('Mounting reducer','Mounting reducer','Mounting reducer',
(#19639));
#19646=PRODUCT('Mounting reducer (1)','Mounting reducer (1)',
'Mounting reducer (1)',(#19639));
#19647=PRODUCT('Mounting reducer (2)','Mounting reducer (2)',
'Mounting reducer (2)',(#19639));
#19648=PRODUCT('Mounting reducer (3)','Mounting reducer (3)',
'Mounting reducer (3)',(#19639));
#19649=PRODUCT('Motor bracket','Motor bracket','Motor bracket',(#19639));
#19650=PRODUCT('Motor envelope','Motor envelope','Motor envelope',(#19639));
#19651=PRODUCT('M3x10 motor screw','M3x10 motor screw',
'M3x10 motor screw',(#19639));
#19652=PRODUCT('M3x10 motor screw (1)','M3x10 motor screw (1)',
'M3x10 motor screw (1)',(#19639));
#19653=PRODUCT('M3x10 motor screw (2)','M3x10 motor screw (2)',
'M3x10 motor screw (2)',(#19639));
#19654=PRODUCT('M3x10 motor screw (3)','M3x10 motor screw (3)',
'M3x10 motor screw (3)',(#19639));
#19655=PRODUCT('Pillow Block Bearing - 12 mm Bore',
'Pillow Block Bearing - 12 mm Bore','Pillow Block Bearing - 12 mm Bore',
(#19639));
#19656=PRODUCT('Housing','Housing','Housing',(#19639));
#19657=PRODUCT('Insert bearing','Insert bearing','Insert bearing',(#19639));
#19658=PRODUCT('Flat Washer - M8','Flat Washer - M8','Flat Washer - M8',
(#19639));
#19659=PRODUCT('M8x25 Bolt','M8x25 Bolt','M8x25 Bolt',(#19639));
#19660=PRODUCT('M5x14 Cap Screw','M5x14 Cap Screw','M5x14 Cap Screw',(#19639));
#19661=PRODUCT('Coupled rotor','Coupled rotor','Coupled rotor',(#19639));
#19662=PRODUCT('Driven shaft','Driven shaft','Driven shaft',(#19639));
#19663=PRODUCT('Motor rotor shaft','Motor rotor shaft',
'Motor rotor shaft',(#19639));
#19664=PRODUCT('Motor shaft adapter','Motor shaft adapter',
'Motor shaft adapter',(#19639));
#19665=PRODUCT('Flywheel','Flywheel','Flywheel',(#19639));
#19666=PRODUCT('Shaft collar','Shaft collar','Shaft collar',(#19639));
#19667=PRODUCT('Shaft collar (1)','Shaft collar (1)','Shaft collar (1)',(#19639));
#19668=PRODUCT('Shaft end keeper','Shaft end keeper','Shaft end keeper',
(#19639));
#19669=PRODUCT('Socket Set Screw - M4x6','Socket Set Screw - M4x6',
'Socket Set Screw - M4x6',(#19639));
#19670=PRODUCT('Flexible Jaw Coupling - 12 mm Bores',
'Flexible Jaw Coupling - 12 mm Bores',
'Flexible Jaw Coupling - 12 mm Bores',(#19639));
#19671=PRODUCT('Hub A','Hub A','Hub A',(#19639));
#19672=PRODUCT('Hub B','Hub B','Hub B',(#19639));
#19673=PRODUCT('Spider','Spider','Spider',(#19639));
#19674=PRODUCT('Parallel Key - 4x4x20','Parallel Key - 4x4x20',
'Parallel Key - 4x4x20',(#19639));
#19675=PRODUCT('Socket Set Screw - M5x8','Socket Set Screw - M5x8',
'Socket Set Screw - M5x8',(#19639));
#19676=PRODUCT('Cap Screw - M4x16','Cap Screw - M4x16',
'Cap Screw - M4x16',(#19639));
#19677=PRESENTATION_STYLE_ASSIGNMENT((#19683));
#19678=PRESENTATION_STYLE_ASSIGNMENT((#19684));
#19679=PRESENTATION_STYLE_ASSIGNMENT((#19685));
#19680=PRESENTATION_STYLE_ASSIGNMENT((#19686));
#19681=PRESENTATION_STYLE_ASSIGNMENT((#19687));
#19682=PRESENTATION_STYLE_ASSIGNMENT((#19688));
#19683=SURFACE_STYLE_USAGE(.BOTH.,#19689);
#19684=SURFACE_STYLE_USAGE(.BOTH.,#19690);
#19685=SURFACE_STYLE_USAGE(.BOTH.,#19691);
#19686=SURFACE_STYLE_USAGE(.BOTH.,#19692);
#19687=SURFACE_STYLE_USAGE(.BOTH.,#19693);
#19688=SURFACE_STYLE_USAGE(.BOTH.,#19694);
#19689=SURFACE_SIDE_STYLE('',(#19695));
#19690=SURFACE_SIDE_STYLE('',(#19696));
#19691=SURFACE_SIDE_STYLE('',(#19697));
#19692=SURFACE_SIDE_STYLE('',(#19698));
#19693=SURFACE_SIDE_STYLE('',(#19699));
#19694=SURFACE_SIDE_STYLE('',(#19700));
#19695=SURFACE_STYLE_FILL_AREA(#19701);
#19696=SURFACE_STYLE_FILL_AREA(#19702);
#19697=SURFACE_STYLE_FILL_AREA(#19703);
#19698=SURFACE_STYLE_FILL_AREA(#19704);
#19699=SURFACE_STYLE_FILL_AREA(#19705);
#19700=SURFACE_STYLE_FILL_AREA(#19706);
#19701=FILL_AREA_STYLE('Steel - Satin',(#19707));
#19702=FILL_AREA_STYLE('CAD Library Painted - Deep blue',(#19708));
#19703=FILL_AREA_STYLE('CAD Library Painted - Graphite',(#19709));
#19704=FILL_AREA_STYLE('CAD Library Painted - Engineering blue',(#19710));
#19705=FILL_AREA_STYLE('CAD Library Painted - Steel gray',(#19711));
#19706=FILL_AREA_STYLE('CAD Library Painted - Light blue',(#19712));
#19707=FILL_AREA_STYLE_COLOUR('Steel - Satin',#19713);
#19708=FILL_AREA_STYLE_COLOUR('CAD Library Painted - Deep blue',#19714);
#19709=FILL_AREA_STYLE_COLOUR('CAD Library Painted - Graphite',#19715);
#19710=FILL_AREA_STYLE_COLOUR('CAD Library Painted - Engineering blue',
#19716);
#19711=FILL_AREA_STYLE_COLOUR('CAD Library Painted - Steel gray',#19717);
#19712=FILL_AREA_STYLE_COLOUR('CAD Library Painted - Light blue',#19718);
#19713=COLOUR_RGB('Steel - Satin',0.627450980392157,0.627450980392157,0.627450980392157);
#19714=COLOUR_RGB('CAD Library Painted - Deep blue',0.0784313725490196,
0.203921568627451,0.349019607843137);
#19715=COLOUR_RGB('CAD Library Painted - Graphite',0.168627450980392,0.192156862745098,
0.231372549019608);
#19716=COLOUR_RGB('CAD Library Painted - Engineering blue',0.12156862745098,
0.356862745098039,0.6);
#19717=COLOUR_RGB('CAD Library Painted - Steel gray',0.592156862745098,
0.631372549019608,0.67843137254902);
#19718=COLOUR_RGB('CAD Library Painted - Light blue',0.286274509803922,
0.552941176470588,0.780392156862745);
#19719=COLOUR_RGB('Dark Blue',0.08,0.2,0.34);
#19720=FILL_AREA_STYLE_COLOUR('',#19719);
#19721=FILL_AREA_STYLE('',(#19720));
#19722=SURFACE_STYLE_FILL_AREA(#19721);
#19723=SURFACE_SIDE_STYLE('',(#19722));
#19724=SURFACE_STYLE_USAGE(.BOTH.,#19723);
#19725=PRESENTATION_STYLE_ASSIGNMENT((#19724));
#19726=COLOUR_RGB('Light Blue',0.38,0.62,0.78);
#19727=FILL_AREA_STYLE_COLOUR('',#19726);
#19728=FILL_AREA_STYLE('',(#19727));
#19729=SURFACE_STYLE_FILL_AREA(#19728);
#19730=SURFACE_SIDE_STYLE('',(#19729));
#19731=SURFACE_STYLE_USAGE(.BOTH.,#19730);
#19732=PRESENTATION_STYLE_ASSIGNMENT((#19731));
#19733=COLOUR_RGB('Sky Blue',0.24,0.69,0.87);
#19734=FILL_AREA_STYLE_COLOUR('',#19733);
#19735=FILL_AREA_STYLE('',(#19734));
#19736=SURFACE_STYLE_FILL_AREA(#19735);
#19737=SURFACE_SIDE_STYLE('',(#19736));
#19738=SURFACE_STYLE_USAGE(.BOTH.,#19737);
#19739=PRESENTATION_STYLE_ASSIGNMENT((#19738));
#19740=COLOUR_RGB('Grey',0.48,0.52,0.57);
#19741=FILL_AREA_STYLE_COLOUR('',#19740);
#19742=FILL_AREA_STYLE('',(#19741));
#19743=SURFACE_STYLE_FILL_AREA(#19742);
#19744=SURFACE_SIDE_STYLE('',(#19743));
#19745=SURFACE_STYLE_USAGE(.BOTH.,#19744);
#19746=PRESENTATION_STYLE_ASSIGNMENT((#19745));
#19747=COLOUR_RGB('Black',0.12,0.14,0.17);
#19748=FILL_AREA_STYLE_COLOUR('',#19747);
#19749=FILL_AREA_STYLE('',(#19748));
#19750=SURFACE_STYLE_FILL_AREA(#19749);
#19751=SURFACE_SIDE_STYLE('',(#19750));
#19752=SURFACE_STYLE_USAGE(.BOTH.,#19751);
#19753=PRESENTATION_STYLE_ASSIGNMENT((#19752));
#19754=COLOUR_RGB('Off White',0.89,0.88,0.83);
#19755=FILL_AREA_STYLE_COLOUR('',#19754);
#19756=FILL_AREA_STYLE('',(#19755));
#19757=SURFACE_STYLE_FILL_AREA(#19756);
#19758=SURFACE_SIDE_STYLE('',(#19757));
#19759=SURFACE_STYLE_USAGE(.BOTH.,#19758);
#19760=PRESENTATION_STYLE_ASSIGNMENT((#19759));
ENDSEC;
END-ISO-10303-21;
